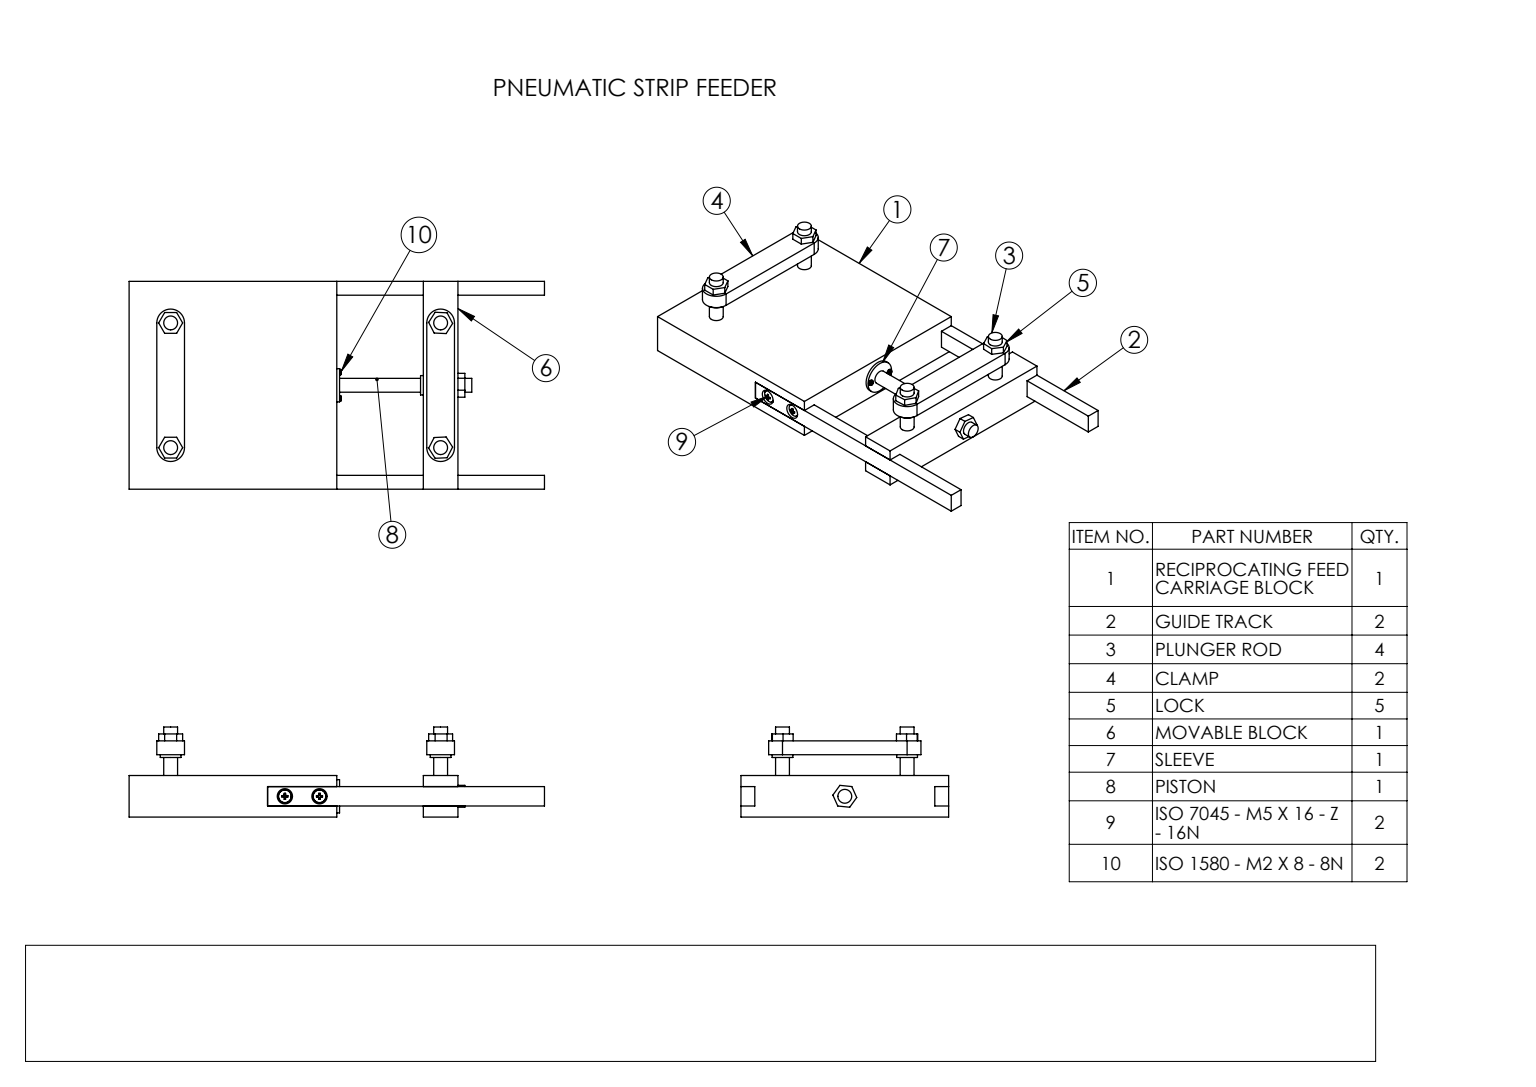
ISO-10303-21;
HEADER;
FILE_DESCRIPTION (('STEP AP214'),
    '1' );
FILE_NAME ('MAS-179',
    '2026-10-27T14:18:53',
    ( '' ),
    ( '' ),
    'SwSTEP 2.0',
    'SolidWorks 2026',
    '' );
FILE_SCHEMA (( 'AUTOMOTIVE_DESIGN' ));
ENDSEC;

DATA;
#1 = DIRECTION ( 'NONE',  ( -1.000000000000000000, -0.000000000000000000, -0.000000000000000000 ) ) ;
#2 = PLANE ( 'NONE',  #2825 ) ;
#3 = LINE ( 'NONE', #3246, #2138 ) ;
#4 = EDGE_LOOP ( 'NONE', ( #1502, #1673, #5385 ) ) ;
#5 = DIRECTION ( 'NONE',  ( -0.02052338132068530496, 0.000000000000000000, 0.9997893732277642886 ) ) ;
#6 = FACE_BOUND ( 'NONE', #2071, .T. ) ;
#7 = AXIS2_PLACEMENT_3D ( 'NONE', #5540, #5177, #924 ) ;
#8 = CARTESIAN_POINT ( 'NONE',  ( 2.740000000000000213, -0.9838866223905674557, -0.5150000000000000133 ) ) ;
#9 = CIRCLE ( 'NONE', #2713, 2.649999999999999467 ) ;
#10 = FACE_OUTER_BOUND ( 'NONE', #5268, .T. ) ;
#11 = COLOUR_RGB ( '',0.8941176470588234615, 0.8941176470588234615, 0.8941176470588234615 ) ;
#12 = AXIS2_PLACEMENT_3D ( 'NONE', #3102, #281, #5829 ) ;
#13 = EDGE_LOOP ( 'NONE', ( #5766, #2705, #5746, #232 ) ) ;
#14 = CARTESIAN_POINT ( 'NONE',  ( 0.000000000000000000, -2.349999999999999201, -0.5150000000000000133 ) ) ;
#15 = CONTEXT_DEPENDENT_SHAPE_REPRESENTATION ( #3045, #4270 ) ;
#16 = AXIS2_PLACEMENT_3D ( 'NONE', #3293, #3357, #1408 ) ;
#17 = DIRECTION ( 'NONE',  ( 1.000000000000000000, -0.000000000000000000, -0.000000000000000000 ) ) ;
#18 = ORIENTED_EDGE ( 'NONE', *, *, #5131, .T. ) ;
#19 = DIRECTION ( 'NONE',  ( 0.8571673013836870192, 1.049727191973306873E-16, -0.5150380737757234151 ) ) ;
#20 = ADVANCED_FACE ( 'NONE', ( #1293 ), #2022, .F. ) ;
#21 = VECTOR ( 'NONE', #291, 1000.000000000000000 ) ;
#22 = EDGE_LOOP ( 'NONE', ( #259, #3713, #2794, #1342 ) ) ;
#23 = ADVANCED_FACE ( 'NONE', ( #3966 ), #1603, .F. ) ;
#24 = ORIENTED_EDGE ( 'NONE', *, *, #4586, .F. ) ;
#25 = CIRCLE ( 'NONE', #2627, 2.500000000000002220 ) ;
#26 = EDGE_CURVE ( 'NONE', #2563, #1725, #4179, .T. ) ;
#27 = TOROIDAL_SURFACE ( 'NONE', #1462, 4.300000000000001599, 0.4499999999999985678 ) ;
#28 = DIRECTION ( 'NONE',  ( 1.000000000000000000, -0.000000000000000000, -0.000000000000000000 ) ) ;
#29 = CARTESIAN_POINT ( 'NONE',  ( 19.70000000000000284, 2.500000000000000000, 0.000000000000000000 ) ) ;
#30 = CARTESIAN_POINT ( 'NONE',  ( 25.00000000000000711, 7.000000000000011546, 65.00000000000000000 ) ) ;
#31 = CARTESIAN_POINT ( 'NONE',  ( 137.4999999999999716, -7.000000000000013323, 75.00000000000001421 ) ) ;
#32 = EDGE_LOOP ( 'NONE', ( #2166, #2925, #468, #4500 ) ) ;
#33 = CIRCLE ( 'NONE', #3411, 2.500000000000002220 ) ;
#34 = VECTOR ( 'NONE', #480, 1000.000000000000000 ) ;
#35 = FILL_AREA_STYLE ('',( #3774 ) ) ;
#36 = CARTESIAN_POINT ( 'NONE',  ( 2.740000000000000213, 0.000000000000000000, 0.8509999999999999787 ) ) ;
#37 = AXIS2_PLACEMENT_3D ( 'NONE', #854, #5957, #5527 ) ;
#38 = SPHERICAL_SURFACE ( 'NONE', #3792, 8.000000000000000000 ) ;
#39 = EDGE_CURVE ( 'NONE', #3671, #1708, #102, .T. ) ;
#40 = MECHANICAL_DESIGN_GEOMETRIC_PRESENTATION_REPRESENTATION (  '', ( #808 ), #5082 ) ;
#41 = ORIENTED_EDGE ( 'NONE', *, *, #5391, .F. ) ;
#42 = DIRECTION ( 'NONE',  ( -1.000000000000000000, -0.000000000000000000, -0.000000000000000000 ) ) ;
#43 = AXIS2_PLACEMENT_3D ( 'NONE', #4617, #1390, #1920 ) ;
#44 = ORIENTED_EDGE ( 'NONE', *, *, #2648, .T. ) ;
#45 = CARTESIAN_POINT ( 'NONE',  ( 55.00000000000000711, 0.000000000000000000, 0.000000000000000000 ) ) ;
#46 = CARTESIAN_POINT ( 'NONE',  ( 0.3226060873438392207, -0.5150000000000068967, 2.189154565102729766 ) ) ;
#47 = ITEM_DEFINED_TRANSFORMATION ( 'NONE', 'NONE', #4502,  #5080 ) ;
#48 = SURFACE_STYLE_USAGE ( .BOTH. , #917 ) ;
#49 = EDGE_LOOP ( 'NONE', ( #4386, #5805, #654, #4968 ) ) ;
#50 = DIRECTION ( 'NONE',  ( -1.000000000000000000, -0.000000000000000000, -0.000000000000000000 ) ) ;
#51 = VERTEX_POINT ( 'NONE', #4696 ) ;
#52 = VERTEX_POINT ( 'NONE', #526 ) ;
#53 =( NAMED_UNIT ( * ) PLANE_ANGLE_UNIT ( ) SI_UNIT ( $, .RADIAN. ) );
#54 = CARTESIAN_POINT ( 'NONE',  ( 0.000000000000000000, 0.000000000000000000, 75.00000000000000000 ) ) ;
#55 = EDGE_CURVE ( 'NONE', #1875, #2958, #1837, .T. ) ;
#56 = CARTESIAN_POINT ( 'NONE',  ( -45.00000000000002842, 0.000000000000000000, -49.99999999999998579 ) ) ;
#57 = DIRECTION ( 'NONE',  ( 0.000000000000000000, 0.000000000000000000, -1.000000000000000000 ) ) ;
#58 = PRODUCT ( 'Reciprocating Feed Carriage Block', 'Reciprocating Feed Carriage Block', '', ( #3675 ) ) ;
#59 = DIRECTION ( 'NONE',  ( 0.000000000000000000, 0.000000000000000000, 1.000000000000000000 ) ) ;
#60 = VERTEX_POINT ( 'NONE', #3659 ) ;
#61 = ADVANCED_FACE ( 'NONE', ( #5096 ), #2836, .F. ) ;
#62 = CARTESIAN_POINT ( 'NONE',  ( 0.000000000000000000, 0.000000000000000000, 0.000000000000000000 ) ) ;
#63 = DIRECTION ( 'NONE',  ( 0.000000000000000000, 1.000000000000000000, 3.280956645156627724E-15 ) ) ;
#64 =( REPRESENTATION_RELATIONSHIP ('NONE','NONE', #5609, #5016 ) REPRESENTATION_RELATIONSHIP_WITH_TRANSFORMATION ( #5642 )SHAPE_REPRESENTATION_RELATIONSHIP( ) );
#65 = AXIS2_PLACEMENT_3D ( 'NONE', #2300, #5491, #4094 ) ;
#66 = DIRECTION ( 'NONE',  ( 1.000000000000000000, 0.000000000000000000, 0.000000000000000000 ) ) ;
#67 = ORIENTED_EDGE ( 'NONE', *, *, #3505, .F. ) ;
#68 =( NAMED_UNIT ( * ) SI_UNIT ( $, .STERADIAN. ) SOLID_ANGLE_UNIT ( ) );
#69 = LINE ( 'NONE', #156, #3339 ) ;
#70 = ADVANCED_FACE ( 'NONE', ( #1406 ), #469, .F. ) ;
#71 = AXIS2_PLACEMENT_3D ( 'NONE', #3867, #5717, #1567 ) ;
#72 = EDGE_LOOP ( 'NONE', ( #5163, #1445, #4342, #1553 ) ) ;
#73 = CARTESIAN_POINT ( 'NONE',  ( 2.740000000000000213, 0.000000000000000000, 0.000000000000000000 ) ) ;
#74 = CARTESIAN_POINT ( 'NONE',  ( -25.39999999999996305, 0.000000000000000000, 0.000000000000000000 ) ) ;
#75 = LINE ( 'NONE', #5584, #2218 ) ;
#76 = CARTESIAN_POINT ( 'NONE',  ( 24.99999999999998224, 6.999999999999985789, 65.00000000000000000 ) ) ;
#77 = ORIENTED_EDGE ( 'NONE', *, *, #5201, .F. ) ;
#78 = ORIENTED_EDGE ( 'NONE', *, *, #4185, .T. ) ;
#79 = PRESENTATION_STYLE_ASSIGNMENT (( #620 ) ) ;
#80 = DIRECTION ( 'NONE',  ( 0.000000000000000000, 1.000000000000000000, -0.000000000000000000 ) ) ;
#81 = ORIENTED_EDGE ( 'NONE', *, *, #5316, .T. ) ;
#82 = DIRECTION ( 'NONE',  ( -1.000000000000000000, -0.000000000000000000, -0.000000000000000000 ) ) ;
#83 = DIRECTION ( 'NONE',  ( 0.000000000000000000, 1.000000000000000000, 0.000000000000000000 ) ) ;
#84 = DIRECTION ( 'NONE',  ( 0.000000000000000000, 0.000000000000000000, 1.000000000000000000 ) ) ;
#85 = ORIENTED_EDGE ( 'NONE', *, *, #3683, .T. ) ;
#86 =( NAMED_UNIT ( * ) PLANE_ANGLE_UNIT ( ) SI_UNIT ( $, .RADIAN. ) );
#87 = DIRECTION ( 'NONE',  ( -0.000000000000000000, -1.000000000000000000, -0.000000000000000000 ) ) ;
#88 = CIRCLE ( 'NONE', #5797, 5.000000000000004441 ) ;
#89 = CARTESIAN_POINT ( 'NONE',  ( -55.00000000000001421, 40.00000000000000000, -45.00000000000000000 ) ) ;
#90 = CARTESIAN_POINT ( 'NONE',  ( 75.00000000000001421, 0.000000000000000000, 0.000000000000000000 ) ) ;
#91 = ADVANCED_FACE ( 'NONE', ( #3214 ), #1319, .F. ) ;
#92 = ORIENTED_EDGE ( 'NONE', *, *, #3018, .T. ) ;
#93 = ADVANCED_FACE ( 'NONE', ( #1832 ), #5149, .T. ) ;
#94 = VERTEX_POINT ( 'NONE', #863 ) ;
#95 = DIRECTION ( 'NONE',  ( -0.000000000000000000, -0.000000000000000000, 1.000000000000000000 ) ) ;
#96 = AXIS2_PLACEMENT_3D ( 'NONE', #2644, #2066, #2156 ) ;
#97 = EDGE_CURVE ( 'NONE', #4020, #2197, #3211, .T. ) ;
#98 = VECTOR ( 'NONE', #2286, 1000.000000000000000 ) ;
#99 = EDGE_LOOP ( 'NONE', ( #5298, #5545, #3236, #2859 ) ) ;
#100 = FACE_OUTER_BOUND ( 'NONE', #830, .T. ) ;
#101 = CARTESIAN_POINT ( 'NONE',  ( 0.06760930072668806801, -4.837354856632045452E-15, 0.000000000000000000 ) ) ;
#102 = CIRCLE ( 'NONE', #5140, 2.500000000000002220 ) ;
#103 = CARTESIAN_POINT ( 'NONE',  ( 1.424271237134740131, 0.000000000000000000, 0.000000000000000000 ) ) ;
#104 = SURFACE_STYLE_FILL_AREA ( #4777 ) ;
#105 = VERTEX_POINT ( 'NONE', #4634 ) ;
#106 = EDGE_CURVE ( 'NONE', #5742, #4738, #1545, .T. ) ;
#107 = VERTEX_POINT ( 'NONE', #2804 ) ;
#108 = AXIS2_PLACEMENT_3D ( 'NONE', #1468, #5154, #2894 ) ;
#109 = LINE ( 'NONE', #3376, #1061 ) ;
#110 = CARTESIAN_POINT ( 'NONE',  ( 7.345657149124971141, -1.312408941149200814, 2.762944903268657774E-16 ) ) ;
#111 = VERTEX_POINT ( 'NONE', #3686 ) ;
#112 = VECTOR ( 'NONE', #1206, 1000.000000000000000 ) ;
#113 = AXIS2_PLACEMENT_3D ( 'NONE', #2260, #4112, #2193 ) ;
#114 = FACE_OUTER_BOUND ( 'NONE', #3648, .T. ) ;
#115 = DIRECTION ( 'NONE',  ( -0.000000000000000000, -0.000000000000000000, 1.000000000000000000 ) ) ;
#116 = DIRECTION ( 'NONE',  ( 1.000000000000000000, -0.000000000000000000, -0.000000000000000000 ) ) ;
#117 = EDGE_LOOP ( 'NONE', ( #4692, #1220, #1894, #1366 ) ) ;
#118 = VECTOR ( 'NONE', #5034, 1000.000000000000000 ) ;
#119 = VECTOR ( 'NONE', #946, 1000.000000000000000 ) ;
#120 = FACE_BOUND ( 'NONE', #3180, .T. ) ;
#121 = DIRECTION ( 'NONE',  ( -1.000000000000000000, 0.000000000000000000, 0.000000000000000000 ) ) ;
#122 = CARTESIAN_POINT ( 'NONE',  ( 135.4999999999999716, 0.000000000000000000, 0.000000000000000000 ) ) ;
#123 = CIRCLE ( 'NONE', #1373, 0.8509999999999999787 ) ;
#125 = CIRCLE ( 'NONE', #3997, 7.000000000000000000 ) ;
#124 = DIRECTION ( 'NONE',  ( 0.000000000000000000, 0.000000000000000000, -1.000000000000000000 ) ) ;
#126 = MANIFOLD_SOLID_BREP ( 'Boss-Extrude2', #2558 ) ;
#127 = EDGE_LOOP ( 'NONE', ( #1000, #825, #2890, #4264 ) ) ;
#128 = VERTEX_POINT ( 'NONE', #4177 ) ;
#129 = DIRECTION ( 'NONE',  ( -0.000000000000000000, -1.000000000000000000, -0.000000000000000000 ) ) ;
#130 = EDGE_CURVE ( 'NONE', #4142, #1478, #3633, .T. ) ;
#131 = EDGE_CURVE ( 'NONE', #60, #666, #9, .T. ) ;
#132 = COLOUR_RGB ( '',1.000000000000000000, 0.9490196078431372140, 0.9098039215686274384 ) ;
#133 = ORIENTED_EDGE ( 'NONE', *, *, #2992, .F. ) ;
#134 = CARTESIAN_POINT ( 'NONE',  ( 77.00000000000001421, 0.000000000000000000, -9.500000000000000000 ) ) ;
#135 = EDGE_CURVE ( 'NONE', #2028, #5067, #3489, .T. ) ;
#136 = CARTESIAN_POINT ( 'NONE',  ( 2.740000000000000213, 0.000000000000000000, 0.000000000000000000 ) ) ;
#137 = CARTESIAN_POINT ( 'NONE',  ( 0.5000000000000000000, 0.2499999999999982792, 2.000000000000001776 ) ) ;
#138 = CYLINDRICAL_SURFACE ( 'NONE', #1374, 5.000000000000004441 ) ;
#139 = EDGE_LOOP ( 'NONE', ( #819, #2768, #3895, #5842 ) ) ;
#140 = VERTEX_POINT ( 'NONE', #4746 ) ;
#141 = EDGE_CURVE ( 'NONE', #5390, #1345, #2004, .T. ) ;
#142 = CARTESIAN_POINT ( 'NONE',  ( 2.740000000000000213, -0.9838866223905676778, 0.5149999999999995692 ) ) ;
#143 = CARTESIAN_POINT ( 'NONE',  ( 0.06760930072668894231, -0.9010842325122859764, 0.5149999999999992362 ) ) ;
#144 = LINE ( 'NONE', #4359, #211 ) ;
#145 = LINE ( 'NONE', #3381, #4186 ) ;
#146 = ORIENTED_EDGE ( 'NONE', *, *, #1899, .T. ) ;
#147 = CLOSED_SHELL ( 'NONE', ( #248, #2661, #5068, #1341, #3720, #5571, #3327, #1429, #4479, #1422, #4024 ) ) ;
#148 = APPLICATION_PROTOCOL_DEFINITION ( 'draft international standard', 'automotive_design', 1998, #5751 ) ;
#149 = CARTESIAN_POINT ( 'NONE',  ( 2.740000000000000213, 0.000000000000000000, 0.000000000000000000 ) ) ;
#150 = DIRECTION ( 'NONE',  ( 0.000000000000000000, 1.000000000000000000, 0.000000000000000000 ) ) ;
#151 = CARTESIAN_POINT ( 'NONE',  ( 75.00000000000001421, 1.224646799147354440E-16, -8.500000000000000000 ) ) ;
#152 = DIRECTION ( 'NONE',  ( -0.000000000000000000, -1.000000000000000000, -0.000000000000000000 ) ) ;
#153 = DIRECTION ( 'NONE',  ( 0.000000000000000000, 0.000000000000000000, 1.000000000000000000 ) ) ;
#154 = EDGE_LOOP ( 'NONE', ( #4564, #1318, #947, #4844 ) ) ;
#155 = ORIENTED_EDGE ( 'NONE', *, *, #5293, .T. ) ;
#156 = CARTESIAN_POINT ( 'NONE',  ( 2.740000000000000213, 0.5150000000000035660, -0.9838866223905657904 ) ) ;
#157 = UNCERTAINTY_MEASURE_WITH_UNIT (LENGTH_MEASURE( 1.000000000000000082E-05 ), #285, 'distance_accuracy_value', 'NONE');
#158 = ORIENTED_EDGE ( 'NONE', *, *, #2741, .F. ) ;
#159 = EDGE_CURVE ( 'NONE', #4312, #626, #169, .T. ) ;
#160 = CARTESIAN_POINT ( 'NONE',  ( 0.6000000000000000888, 0.000000000000000000, 0.000000000000000000 ) ) ;
#161 = CARTESIAN_POINT ( 'NONE',  ( 0.5000000000000000000, 0.2499999999999982792, -2.000000000000000000 ) ) ;
#162 = CONTEXT_DEPENDENT_SHAPE_REPRESENTATION ( #64, #5291 ) ;
#163 = DIRECTION ( 'NONE',  ( 1.000000000000000000, 0.000000000000000000, 0.000000000000000000 ) ) ;
#164 = PRODUCT_RELATED_PRODUCT_CATEGORY ( 'part', '', ( #1927 ) ) ;
#165 = DIRECTION ( 'NONE',  ( 0.000000000000000000, 0.000000000000000000, 1.000000000000000000 ) ) ;
#166 = ORIENTED_EDGE ( 'NONE', *, *, #2504, .F. ) ;
#167 = ORIENTED_EDGE ( 'NONE', *, *, #1148, .F. ) ;
#168 = ADVANCED_FACE ( 'NONE', ( #2861 ), #5707, .F. ) ;
#169 = LINE ( 'NONE', #5681, #675 ) ;
#170 = DIRECTION ( 'NONE',  ( 1.000000000000000000, 0.000000000000000000, 0.000000000000000000 ) ) ;
#171 = VERTEX_POINT ( 'NONE', #3409 ) ;
#172 = DIRECTION ( 'NONE',  ( 0.000000000000000000, 0.000000000000000000, -1.000000000000000000 ) ) ;
#173 = DIRECTION ( 'NONE',  ( -1.000000000000000000, -0.000000000000000000, -0.000000000000000000 ) ) ;
#174 = DIRECTION ( 'NONE',  ( 0.8949343913984706411, 1.487067055422294855E-15, -0.4461977533473793223 ) ) ;
#175 = ORIENTED_EDGE ( 'NONE', *, *, #2979, .F. ) ;
#176 = EDGE_CURVE ( 'NONE', #2634, #3745, #5619, .T. ) ;
#177 = DIRECTION ( 'NONE',  ( 0.9997893732277642886, 0.000000000000000000, -0.02052338132068530496 ) ) ;
#178 = CARTESIAN_POINT ( 'NONE',  ( -53.66025403784439618, 45.00000000000000000, 45.00000000000001421 ) ) ;
#179 = DIRECTION ( 'NONE',  ( 1.000000000000000000, 0.000000000000000000, 0.000000000000000000 ) ) ;
#180 = PLANE ( 'NONE',  #2511 ) ;
#181 = DIRECTION ( 'NONE',  ( 0.000000000000000000, 0.000000000000000000, 1.000000000000000000 ) ) ;
#182 = DIRECTION ( 'NONE',  ( -0.8949343913984706411, 0.4461977533473793223, 0.000000000000000000 ) ) ;
#183 = ORIENTED_EDGE ( 'NONE', *, *, #1823, .F. ) ;
#184 = EDGE_LOOP ( 'NONE', ( #1736, #1918, #2803, #4807 ) ) ;
#185 = AXIS2_PLACEMENT_3D ( 'NONE', #3101, #5825, #5378 ) ;
#186 = DIRECTION ( 'NONE',  ( 0.000000000000000000, 0.000000000000000000, -1.000000000000000000 ) ) ;
#187 = EDGE_LOOP ( 'NONE', ( #1142, #4922, #3638, #5470 ) ) ;
#188=STYLED_ITEM('',(#6006),#2182);
#189 = MANIFOLD_SOLID_BREP ( 'RecessCore', #1492 ) ;
#190 = DIRECTION ( 'NONE',  ( 1.000000000000000000, 0.000000000000000000, 0.000000000000000000 ) ) ;
#191 = CARTESIAN_POINT ( 'NONE',  ( 137.4999999999999716, 15.00000000000000000, 75.00000000000001421 ) ) ;
#192 = ORIENTED_EDGE ( 'NONE', *, *, #4630, .T. ) ;
#193 = ORIENTED_EDGE ( 'NONE', *, *, #1729, .T. ) ;
#194 =( NAMED_UNIT ( * ) SI_UNIT ( $, .STERADIAN. ) SOLID_ANGLE_UNIT ( ) );
#195 = AXIS2_PLACEMENT_3D ( 'NONE', #2672, #1764, #375 ) ;
#196 = MANIFOLD_SOLID_BREP ( 'M2 Clearance Hole1', #4902 ) ;
#197 = CARTESIAN_POINT ( 'NONE',  ( 37.50000000000000711, 6.288372600415927295E-15, 65.00000000000000000 ) ) ;
#198 = EDGE_CURVE ( 'NONE', #4039, #4278, #109, .T. ) ;
#199 = VERTEX_POINT ( 'NONE', #3354 ) ;
#200 = DIRECTION ( 'NONE',  ( -1.000000000000000000, 2.312964634635742895E-17, 0.000000000000000000 ) ) ;
#201 = ADVANCED_FACE ( 'NONE', ( #5199 ), #2031, .F. ) ;
#202 = FACE_OUTER_BOUND ( 'NONE', #385, .T. ) ;
#203 = EDGE_CURVE ( 'NONE', #1147, #2495, #5910, .T. ) ;
#204 = PLANE ( 'NONE',  #1558 ) ;
#205 = AXIS2_PLACEMENT_3D ( 'NONE', #3546, #4367, #1077 ) ;
#206 = ORIENTED_EDGE ( 'NONE', *, *, #4724, .F. ) ;
#207 = DIRECTION ( 'NONE',  ( -0.04608749363411584338, 0.000000000000000000, 0.9989374069132286316 ) ) ;
#208 = ADVANCED_FACE ( 'NONE', ( #1064 ), #1706, .F. ) ;
#209 = LINE ( 'NONE', #2049, #935 ) ;
#210 = TOROIDAL_SURFACE ( 'NONE', #5533, 1.336466033005844434, 0.5999999999999999778 ) ;
#211 = VECTOR ( 'NONE', #2932, 1000.000000000000000 ) ;
#212 = CARTESIAN_POINT ( 'NONE',  ( -53.66025403784439618, 45.00000000000000000, 45.00000000000001421 ) ) ;
#213 = CARTESIAN_POINT ( 'NONE',  ( 0.000000000000000000, -2.349999999999997424, 0.5149999999999992362 ) ) ;
#214 = CARTESIAN_POINT ( 'NONE',  ( 137.4999999999999716, 0.000000000000000000, 5.000000000000000000 ) ) ;
#215 = CYLINDRICAL_SURFACE ( 'NONE', #3221, 5.000000000000004441 ) ;
#216 = MANIFOLD_SOLID_BREP ( 'Slot', #3438 ) ;
#217 = ORIENTED_EDGE ( 'NONE', *, *, #5542, .F. ) ;
#218 = AXIS2_PLACEMENT_3D ( 'NONE', #3417, #2963, #2469 ) ;
#219 = ORIENTED_EDGE ( 'NONE', *, *, #1151, .T. ) ;
#220 = LINE ( 'NONE', #1177, #2270 ) ;
#221 = UNCERTAINTY_MEASURE_WITH_UNIT (LENGTH_MEASURE( 1.000000000000000082E-05 ), #1761, 'distance_accuracy_value', 'NONE');
#222 = VECTOR ( 'NONE', #506, 1000.000000000000000 ) ;
#223 = AXIS2_PLACEMENT_3D ( 'NONE', #4631, #50, #5962 ) ;
#224 = EDGE_CURVE ( 'NONE', #3671, #5354, #1284, .T. ) ;
#225 = VERTEX_POINT ( 'NONE', #2651 ) ;
#226 = VECTOR ( 'NONE', #1143, 1000.000000000000000 ) ;
#227 =( NAMED_UNIT ( * ) PLANE_ANGLE_UNIT ( ) SI_UNIT ( $, .RADIAN. ) );
#228 = VECTOR ( 'NONE', #4642, 1000.000000000000000 ) ;
#229 = CYLINDRICAL_SURFACE ( 'NONE', #96, 5.000000000000000000 ) ;
#230 = FACE_BOUND ( 'NONE', #460, .T. ) ;
#231 = ORIENTED_EDGE ( 'NONE', *, *, #2067, .F. ) ;
#232 = ORIENTED_EDGE ( 'NONE', *, *, #1791, .F. ) ;
#233 = EDGE_CURVE ( 'NONE', #2491, #3368, #3007, .T. ) ;
#234 = DIRECTION ( 'NONE',  ( 0.000000000000000000, 1.000000000000000000, 0.000000000000000000 ) ) ;
#235 = EDGE_LOOP ( 'NONE', ( #5621, #519 ) ) ;
#236 = CARTESIAN_POINT ( 'NONE',  ( 3.699999999999998401, 5.817072295949927426E-16, -4.750000000000000000 ) ) ;
#237 = LINE ( 'NONE', #652, #2519 ) ;
#238 = DIRECTION ( 'NONE',  ( 0.000000000000000000, 1.000000000000000000, -0.000000000000000000 ) ) ;
#239 = CIRCLE ( 'NONE', #3046, 1.037871761867652065 ) ;
#240 = ORIENTED_EDGE ( 'NONE', *, *, #1900, .T. ) ;
#241 = SHAPE_DEFINITION_REPRESENTATION ( #544, #4225 ) ;
#242 = FACE_BOUND ( 'NONE', #235, .T. ) ;
#243 = CLOSED_SHELL ( 'NONE', ( #387, #4012, #859, #4445, #3072, #5289, #5765, #2717, #915, #3857, #5172, #2981, #4882, #2867, #4541, #2097, #5257, #5474, #4624, #721, #3860, #288 ) ) ;
#244 = ADVANCED_FACE ( 'NONE', ( #1649 ), #3949, .T. ) ;
#245 = DIRECTION ( 'NONE',  ( 1.000000000000000000, -0.000000000000000000, -0.000000000000000000 ) ) ;
#246 = DIRECTION ( 'NONE',  ( -0.000000000000000000, -0.000000000000000000, -1.000000000000000000 ) ) ;
#247 = LINE ( 'NONE', #2084, #1072 ) ;
#248 = ADVANCED_FACE ( 'NONE', ( #4015 ), #1620, .F. ) ;
#249 = DIRECTION ( 'NONE',  ( -0.000000000000000000, 0.000000000000000000, -1.000000000000000000 ) ) ;
#250 = EDGE_LOOP ( 'NONE', ( #3367, #4044, #762, #2973 ) ) ;
#251 = ORIENTED_EDGE ( 'NONE', *, *, #3575, .F. ) ;
#252 = CARTESIAN_POINT ( 'NONE',  ( -53.66025403784439618, 40.00000000000000000, 45.00000000000001421 ) ) ;
#253 = ORIENTED_EDGE ( 'NONE', *, *, #2086, .T. ) ;
#254 = ADVANCED_FACE ( 'NONE', ( #5836 ), #1248, .F. ) ;
#255 = LINE ( 'NONE', #2124, #1542 ) ;
#256 = APPLICATION_CONTEXT ( 'automotive_design' ) ;
#257 = CARTESIAN_POINT ( 'NONE',  ( 2.740000000000000213, -0.5150000000000022338, 0.6774776749089210792 ) ) ;
#258 = ORIENTED_EDGE ( 'NONE', *, *, #3702, .T. ) ;
#259 = ORIENTED_EDGE ( 'NONE', *, *, #388, .T. ) ;
#260 = CARTESIAN_POINT ( 'NONE',  ( 67.00000000000001421, 6.123233995736766282E-16, 5.000000000000000000 ) ) ;
#261 = ORIENTED_EDGE ( 'NONE', *, *, #932, .T. ) ;
#262 = DIRECTION ( 'NONE',  ( 1.000000000000000000, -0.000000000000000000, -0.000000000000000000 ) ) ;
#263 = LINE ( 'NONE', #1654, #3890 ) ;
#264 = DIRECTION ( 'NONE',  ( -1.000000000000000000, -0.000000000000000000, -0.000000000000000000 ) ) ;
#265 = ORIENTED_EDGE ( 'NONE', *, *, #3879, .F. ) ;
#266 = CARTESIAN_POINT ( 'NONE',  ( 197.0261205246305281, 0.000000000000000000, -87.87824609756007987 ) ) ;
#267 = CARTESIAN_POINT ( 'NONE',  ( 196.6421356237309510, 0.000000000000000000, 5.000000000000000000 ) ) ;
#268 = CYLINDRICAL_SURFACE ( 'NONE', #4477, 2.500000000000002220 ) ;
#269 = DIRECTION ( 'NONE',  ( 0.000000000000000000, 1.000000000000000000, 1.153406566473941260E-16 ) ) ;
#270 = DIRECTION ( 'NONE',  ( -0.000000000000000000, -1.000000000000000000, -0.000000000000000000 ) ) ;
#271 = CARTESIAN_POINT ( 'NONE',  ( 24.99999999999998224, 6.999999999999985789, 75.00000000000000000 ) ) ;
#272 = MANIFOLD_SOLID_BREP ( 'Cut-Extrude2', #243 ) ;
#273 = ORIENTED_EDGE ( 'NONE', *, *, #4438, .F. ) ;
#274 = ORIENTED_EDGE ( 'NONE', *, *, #5318, .F. ) ;
#275 = DIRECTION ( 'NONE',  ( 0.000000000000000000, 0.000000000000000000, 1.000000000000000000 ) ) ;
#276 = ORIENTED_EDGE ( 'NONE', *, *, #2236, .T. ) ;
#277 = ADVANCED_FACE ( 'NONE', ( #3588 ), #323, .T. ) ;
#278 = EDGE_CURVE ( 'NONE', #1461, #3435, #2305, .T. ) ;
#279 = CARTESIAN_POINT ( 'NONE',  ( 19.70000000000000284, 0.000000000000000000, 2.500000000000000000 ) ) ;
#280 = EDGE_CURVE ( 'NONE', #2788, #5831, #1766, .T. ) ;
#281 = DIRECTION ( 'NONE',  ( 1.000000000000000000, 0.000000000000000000, 0.000000000000000000 ) ) ;
#282 = ORIENTED_EDGE ( 'NONE', *, *, #2831, .T. ) ;
#283 = VERTEX_POINT ( 'NONE', #413 ) ;
#284 = PRESENTATION_STYLE_ASSIGNMENT (( #3561 ) ) ;
#285 =( LENGTH_UNIT ( ) NAMED_UNIT ( * ) SI_UNIT ( .MILLI., .METRE. ) );
#286 = ORIENTED_EDGE ( 'NONE', *, *, #1877, .F. ) ;
#287 = CARTESIAN_POINT ( 'NONE',  ( 0.5000000000000000000, 0.000000000000000000, 0.000000000000000000 ) ) ;
#288 = ADVANCED_FACE ( 'NONE', ( #4164 ), #2769, .F. ) ;
#289 = DIRECTION ( 'NONE',  ( 0.000000000000000000, 0.000000000000000000, 1.000000000000000000 ) ) ;
#290 = ORIENTED_EDGE ( 'NONE', *, *, #4030, .T. ) ;
#291 = DIRECTION ( 'NONE',  ( 1.000000000000000000, -3.469446951953614189E-16, -0.000000000000000000 ) ) ;
#292 = EDGE_LOOP ( 'NONE', ( #561, #1118, #3736, #5489 ) ) ;
#293=STYLED_ITEM('',(#6020),#2209);
#294 = ITEM_DEFINED_TRANSFORMATION ( 'NONE', 'NONE', #43,  #5080 ) ;
#295 = CARTESIAN_POINT ( 'NONE',  ( 0.000000000000000000, -0.2499999999999999445, 1.312875263449798879 ) ) ;
#296 = DIRECTION ( 'NONE',  ( 0.000000000000000000, 0.000000000000000000, -1.000000000000000000 ) ) ;
#297 = COLOUR_RGB ( '',0.8941176470588234615, 0.8941176470588234615, 0.8941176470588234615 ) ;
#298 = VECTOR ( 'NONE', #2052, 1000.000000000000227 ) ;
#299 = FACE_OUTER_BOUND ( 'NONE', #2161, .T. ) ;
#300 = DIRECTION ( 'NONE',  ( -1.000000000000000000, -0.000000000000000000, -0.000000000000000000 ) ) ;
#301 = EDGE_CURVE ( 'NONE', #4985, #4357, #4292, .T. ) ;
#302 = CARTESIAN_POINT ( 'NONE',  ( 1.424271237134740131, 0.000000000000000000, 0.000000000000000000 ) ) ;
#303 = ORIENTED_EDGE ( 'NONE', *, *, #3462, .T. ) ;
#304 = MECHANICAL_DESIGN_GEOMETRIC_PRESENTATION_REPRESENTATION (  '', ( #5611 ), #1259 ) ;
#305 = VECTOR ( 'NONE', #5098, 1000.000000000000000 ) ;
#306 = DIRECTION ( 'NONE',  ( 0.000000000000000000, 0.000000000000000000, 1.000000000000000000 ) ) ;
#307 = ORIENTED_EDGE ( 'NONE', *, *, #4245, .F. ) ;
#308 = AXIS2_PLACEMENT_3D ( 'NONE', #4125, #4984, #3159 ) ;
#309 = DIRECTION ( 'NONE',  ( -0.000000000000000000, -1.000000000000000000, -0.000000000000000000 ) ) ;
#310 = PRESENTATION_STYLE_ASSIGNMENT (( #4469 ) ) ;
#311 = ADVANCED_FACE ( 'NONE', ( #2255 ), #3623, .F. ) ;
#312 = DIRECTION ( 'NONE',  ( 1.000000000000000000, 0.000000000000000000, -0.000000000000000000 ) ) ;
#313 = CIRCLE ( 'NONE', #2040, 7.983406227920510467 ) ;
#314 = AXIS2_PLACEMENT_3D ( 'NONE', #3288, #1427, #2751 ) ;
#315 = EDGE_CURVE ( 'NONE', #2436, #2440, #3153, .T. ) ;
#316 = EDGE_CURVE ( 'NONE', #4485, #2436, #3260, .T. ) ;
#317 = CARTESIAN_POINT ( 'NONE',  ( 137.4999999999999716, 15.00000000000000000, 65.00000000000000000 ) ) ;
#318 = AXIS2_PLACEMENT_3D ( 'NONE', #5107, #1395, #3704 ) ;
#319 = VECTOR ( 'NONE', #2665, 1000.000000000000000 ) ;
#321 = ORIENTED_EDGE ( 'NONE', *, *, #1308, .F. ) ;
#320 = EDGE_CURVE ( 'NONE', #2852, #1334, #3202, .T. ) ;
#322 = ORIENTED_EDGE ( 'NONE', *, *, #1089, .F. ) ;
#323 = PLANE ( 'NONE',  #5550 ) ;
#324 = PRESENTATION_LAYER_ASSIGNMENT (  '', '', ( #5551 ) ) ;
#325 = CARTESIAN_POINT ( 'NONE',  ( -45.00000000000001421, 30.00000000000000355, -50.00000000000000000 ) ) ;
#326 = ORIENTED_EDGE ( 'NONE', *, *, #3762, .T. ) ;
#327 = DIRECTION ( 'NONE',  ( 0.000000000000000000, 0.000000000000000000, 1.000000000000000000 ) ) ;
#328 = DIRECTION ( 'NONE',  ( 1.000000000000000000, -0.000000000000000000, -0.000000000000000000 ) ) ;
#329 = EDGE_LOOP ( 'NONE', ( #3488, #1309 ) ) ;
#330 = CARTESIAN_POINT ( 'NONE',  ( 8.300922883092140858E-17, -0.2499999999999997780, -1.455170506525537588 ) ) ;
#331 = ORIENTED_EDGE ( 'NONE', *, *, #2483, .F. ) ;
#332 =( GEOMETRIC_REPRESENTATION_CONTEXT ( 3 ) GLOBAL_UNCERTAINTY_ASSIGNED_CONTEXT ( ( #1483 ) ) GLOBAL_UNIT_ASSIGNED_CONTEXT ( ( #2789, #1481, #68 ) ) REPRESENTATION_CONTEXT ( 'NONE', 'WORKASPACE' ) );
#333 = EDGE_CURVE ( 'NONE', #4738, #5742, #4095, .T. ) ;
#334 = ADVANCED_FACE ( 'NONE', ( #4537 ), #4626, .F. ) ;
#335 = DIRECTION ( 'NONE',  ( -0.8660254037844390407, 0.000000000000000000, -0.4999999999999993894 ) ) ;
#336 = AXIS2_PLACEMENT_3D ( 'NONE', #1876, #5603, #1027 ) ;
#337 = CARTESIAN_POINT ( 'NONE',  ( 2.740000000000000213, -0.5149999999999961275, -0.9838866223905694541 ) ) ;
#338 = AXIS2_PLACEMENT_3D ( 'NONE', #4886, #3449, #2991 ) ;
#339 = DIRECTION ( 'NONE',  ( 1.000000000000000000, 0.000000000000000000, 0.000000000000000000 ) ) ;
#340 = LINE ( 'NONE', #5874, #5255 ) ;
#341 = DIRECTION ( 'NONE',  ( -1.000000000000000000, -0.000000000000000000, -0.000000000000000000 ) ) ;
#342 = VERTEX_POINT ( 'NONE', #46 ) ;
#343 = CARTESIAN_POINT ( 'NONE',  ( 68.00000000000000000, -1.951563910473909559E-15, 75.00000000000000000 ) ) ;
#344 = ORIENTED_EDGE ( 'NONE', *, *, #547, .F. ) ;
#345 = DIRECTION ( 'NONE',  ( -0.000000000000000000, 1.000000000000000000, 1.224646799147353207E-16 ) ) ;
#346 = SHAPE_REPRESENTATION_RELATIONSHIP ( 'NONE' , 'NONE' ,  #2785, #5722 ) ;
#347 = CARTESIAN_POINT ( 'NONE',  ( 2.740000000000000213, 0.9838866223909998876, -0.5150000000000000133 ) ) ;
#348 = FACE_BOUND ( 'NONE', #3880, .T. ) ;
#349 = ADVANCED_FACE ( 'NONE', ( #2746 ), #3674, .F. ) ;
#350 = ORIENTED_EDGE ( 'NONE', *, *, #5483, .F. ) ;
#351 = ORIENTED_EDGE ( 'NONE', *, *, #1899, .F. ) ;
#352 = DIRECTION ( 'NONE',  ( -1.000000000000000000, 0.000000000000000000, 0.000000000000000000 ) ) ;
#353 = DIRECTION ( 'NONE',  ( -0.000000000000000000, -0.000000000000000000, 1.000000000000000000 ) ) ;
#354 = EDGE_LOOP ( 'NONE', ( #2724, #1394 ) ) ;
#355 = CARTESIAN_POINT ( 'NONE',  ( -45.00000000000001421, 40.00000000000000000, 50.00000000000000000 ) ) ;
#356 = CARTESIAN_POINT ( 'NONE',  ( -74.99999999999998579, 15.00000000000000000, 75.00000000000000000 ) ) ;
#357 = ORIENTED_EDGE ( 'NONE', *, *, #4065, .T. ) ;
#358 = DIRECTION ( 'NONE',  ( 0.000000000000000000, 0.000000000000000000, -1.000000000000000000 ) ) ;
#359 = ADVANCED_FACE ( 'NONE', ( #1881 ), #3735, .T. ) ;
#360 = VERTEX_POINT ( 'NONE', #5089 ) ;
#361 = AXIS2_PLACEMENT_3D ( 'NONE', #2845, #4273, #538 ) ;
#362 = DIRECTION ( 'NONE',  ( 0.000000000000000000, 0.000000000000000000, 1.000000000000000000 ) ) ;
#363 = DIRECTION ( 'NONE',  ( 0.000000000000000000, 0.000000000000000000, 1.000000000000000000 ) ) ;
#364 = AXIS2_PLACEMENT_3D ( 'NONE', #2626, #335, #1690 ) ;
#365 = DIRECTION ( 'NONE',  ( -0.000000000000000000, -0.000000000000000000, 1.000000000000000000 ) ) ;
#366 = DIRECTION ( 'NONE',  ( -1.000000000000000000, -0.000000000000000000, -0.000000000000000000 ) ) ;
#367 = EDGE_CURVE ( 'NONE', #1773, #5556, #4512, .T. ) ;
#368 = EDGE_LOOP ( 'NONE', ( #4286, #2908, #2582, #3247 ) ) ;
#369 = CARTESIAN_POINT ( 'NONE',  ( -45.00000000000002842, 15.00000000000000000, -39.99999999999997868 ) ) ;
#370 = ORIENTED_EDGE ( 'NONE', *, *, #3462, .F. ) ;
#371 = DIRECTION ( 'NONE',  ( -1.000000000000000000, -0.000000000000000000, -0.000000000000000000 ) ) ;
#372 = ADVANCED_FACE ( 'NONE', ( #1311 ), #889, .T. ) ;
#373 = FILL_AREA_STYLE ('',( #5951 ) ) ;
#374 = CYLINDRICAL_SURFACE ( 'NONE', #2638, 4.749999999999999112 ) ;
#375 = DIRECTION ( 'NONE',  ( 0.000000000000000000, 0.000000000000000000, -1.000000000000000000 ) ) ;
#376 = EDGE_LOOP ( 'NONE', ( #1948, #3141, #4446, #529, #3460, #5164, #2752, #3738, #499, #1793, #4023, #3829 ) ) ;
#377 = VERTEX_POINT ( 'NONE', #441 ) ;
#378 = CARTESIAN_POINT ( 'NONE',  ( -53.66025403784439618, 45.00000000000000000, 45.00000000000001421 ) ) ;
#379 = ORIENTED_EDGE ( 'NONE', *, *, #3057, .F. ) ;
#380 = DIRECTION ( 'NONE',  ( -3.469446951953614189E-16, -1.000000000000000000, 8.673617379884041635E-17 ) ) ;
#381 = CARTESIAN_POINT ( 'NONE',  ( 150.0000000000000284, 15.00000000000000000, 45.00000000000000000 ) ) ;
#382 = ORIENTED_EDGE ( 'NONE', *, *, #3138, .T. ) ;
#383 = LINE ( 'NONE', #2712, #21 ) ;
#384 = ORIENTED_EDGE ( 'NONE', *, *, #5078, .T. ) ;
#385 = EDGE_LOOP ( 'NONE', ( #2934, #576, #5503, #570 ) ) ;
#386 = VECTOR ( 'NONE', #1556, 1000.000000000000000 ) ;
#387 = ADVANCED_FACE ( 'NONE', ( #827 ), #2284, .F. ) ;
#388 = EDGE_CURVE ( 'NONE', #475, #702, #3140, .T. ) ;
#389 = CARTESIAN_POINT ( 'NONE',  ( 25.00000000000000711, 7.000000000000011546, -75.00000000000000000 ) ) ;
#390 = EDGE_CURVE ( 'NONE', #5094, #2958, #1969, .T. ) ;
#391 = DIRECTION ( 'NONE',  ( -0.000000000000000000, -0.000000000000000000, 1.000000000000000000 ) ) ;
#392 = CARTESIAN_POINT ( 'NONE',  ( 137.4999999999999716, 15.00000000000000000, -75.00000000000000000 ) ) ;
#393 = DIRECTION ( 'NONE',  ( 0.000000000000000000, 0.000000000000000000, -1.000000000000000000 ) ) ;
#394=STYLED_ITEM('',(#6013),#2189);
#395 = EDGE_LOOP ( 'NONE', ( #4054, #2100 ) ) ;
#396 = EDGE_CURVE ( 'NONE', #4357, #4985, #5381, .T. ) ;
#397 = SHAPE_REPRESENTATION_RELATIONSHIP ( 'NONE' , 'NONE' ,  #951, #4058 ) ;
#398 = DIRECTION ( 'NONE',  ( 1.000000000000000000, -0.000000000000000000, -0.000000000000000000 ) ) ;
#399 = AXIS2_PLACEMENT_3D ( 'NONE', #949, #5510, #3267 ) ;
#400 = VECTOR ( 'NONE', #539, 1000.000000000000000 ) ;
#401 = ORIENTED_EDGE ( 'NONE', *, *, #5953, .F. ) ;
#402 = FACE_BOUND ( 'NONE', #4375, .T. ) ;
#403 = AXIS2_PLACEMENT_3D ( 'NONE', #4521, #1, #363 ) ;
#404 = LINE ( 'NONE', #5952, #3410 ) ;
#405 = EDGE_CURVE ( 'NONE', #1403, #3083, #5296, .T. ) ;
#406 = VECTOR ( 'NONE', #2782, 1000.000000000000000 ) ;
#407 = CIRCLE ( 'NONE', #1166, 5.000000000000004441 ) ;
#408 = FACE_BOUND ( 'NONE', #3152, .T. ) ;
#409 = ORIENTED_EDGE ( 'NONE', *, *, #2019, .F. ) ;
#410 = ORIENTED_EDGE ( 'NONE', *, *, #1827, .F. ) ;
#411 = VECTOR ( 'NONE', #264, 1000.000000000000000 ) ;
#412 = CIRCLE ( 'NONE', #978, 5.000000000000004441 ) ;
#413 = CARTESIAN_POINT ( 'NONE',  ( 62.50000000000001421, -1.951563910473909559E-15, -53.49784845693390167 ) ) ;
#414 = DIRECTION ( 'NONE',  ( -1.000000000000000000, -0.000000000000000000, -0.000000000000000000 ) ) ;
#415 = ORIENTED_EDGE ( 'NONE', *, *, #26, .F. ) ;
#416 = AXIS2_PLACEMENT_3D ( 'NONE', #5969, #3664, #3218 ) ;
#417 = VECTOR ( 'NONE', #1999, 1000.000000000000000 ) ;
#418 = FACE_OUTER_BOUND ( 'NONE', #802, .T. ) ;
#419 = DIRECTION ( 'NONE',  ( 0.000000000000000000, 1.000000000000000000, 0.000000000000000000 ) ) ;
#420 = ORIENTED_EDGE ( 'NONE', *, *, #1641, .T. ) ;
#421 = CARTESIAN_POINT ( 'NONE',  ( 0.05011565059742434380, 0.2499999999999982792, -1.595010514166263382 ) ) ;
#422 = EDGE_LOOP ( 'NONE', ( #5932, #2408, #3611, #5800 ) ) ;
#423 = DIRECTION ( 'NONE',  ( -1.000000000000000000, -0.000000000000000000, -0.000000000000000000 ) ) ;
#424 = CARTESIAN_POINT ( 'NONE',  ( -45.00000000000001421, 50.00000000000000000, 50.00000000000000000 ) ) ;
#425 = CARTESIAN_POINT ( 'NONE',  ( 150.0000000000000284, 15.00000000000000000, -49.99999999999998579 ) ) ;
#426 = CARTESIAN_POINT ( 'NONE',  ( 24.99999999999998224, 6.999999999999985789, 75.00000000000000000 ) ) ;
#427 = CYLINDRICAL_SURFACE ( 'NONE', #3498, 5.000000000000004441 ) ;
#428 = ORIENTED_EDGE ( 'NONE', *, *, #4995, .T. ) ;
#429 = ADVANCED_FACE ( 'NONE', ( #3884 ), #4687, .T. ) ;
#430 =( LENGTH_UNIT ( ) NAMED_UNIT ( * ) SI_UNIT ( .MILLI., .METRE. ) );
#431 = CARTESIAN_POINT ( 'NONE',  ( 1.849560077140108394, 0.7556913915602446741, 0.5149999999999996803 ) ) ;
#432 = PRODUCT_DEFINITION_FORMATION_WITH_SPECIFIED_SOURCE ( 'ANY', '', #4798, .NOT_KNOWN. ) ;
#433 = EDGE_LOOP ( 'NONE', ( #3649, #3374, #834, #5095, #5451 ) ) ;
#434 = CARTESIAN_POINT ( 'NONE',  ( -45.00000000000001421, 40.00000000000000000, 39.99999999999999289 ) ) ;
#435 = AXIS2_PLACEMENT_3D ( 'NONE', #5878, #3224, #2274 ) ;
#436 = CARTESIAN_POINT ( 'NONE',  ( 62.50000000000001421, -1.951563910473909559E-15, -65.00000000000000000 ) ) ;
#437 = CARTESIAN_POINT ( 'NONE',  ( 137.4999999999999716, 6.999999999999985789, 75.00000000000000000 ) ) ;
#438 = ORIENTED_EDGE ( 'NONE', *, *, #2529, .F. ) ;
#439 = EDGE_CURVE ( 'NONE', #128, #2057, #2951, .T. ) ;
#440 = EDGE_LOOP ( 'NONE', ( #5310, #2912, #92, #4963 ) ) ;
#441 = CARTESIAN_POINT ( 'NONE',  ( -45.00000000000001421, 40.00000000000000000, 50.00000000000000000 ) ) ;
#442 = ITEM_DEFINED_TRANSFORMATION ( 'NONE', 'NONE', #1093,  #5080 ) ;
#443 = CARTESIAN_POINT ( 'NONE',  ( 2.740000000000000213, -0.5150000000000034550, 0.9838866223909985553 ) ) ;
#444 = ORIENTED_EDGE ( 'NONE', *, *, #5201, .T. ) ;
#445 = DIRECTION ( 'NONE',  ( -0.000000000000000000, -0.000000000000000000, 1.000000000000000000 ) ) ;
#446 = CARTESIAN_POINT ( 'NONE',  ( 0.06760930072668806801, -4.837354856632045452E-15, 0.000000000000000000 ) ) ;
#447 = ORIENTED_EDGE ( 'NONE', *, *, #1010, .T. ) ;
#448 = EDGE_LOOP ( 'NONE', ( #5357, #973 ) ) ;
#449 = PLANE ( 'NONE',  #1541 ) ;
#450 = CARTESIAN_POINT ( 'NONE',  ( 0.3600944671415647891, -0.2500000000000000000, 1.887947737020718941 ) ) ;
#451 = PLANE ( 'NONE',  #1857 ) ;
#452 = DIRECTION ( 'NONE',  ( -0.000000000000000000, -0.000000000000000000, -1.000000000000000000 ) ) ;
#453 = ORIENTED_EDGE ( 'NONE', *, *, #824, .F. ) ;
#454 = FACE_OUTER_BOUND ( 'NONE', #672, .T. ) ;
#455 = FACE_OUTER_BOUND ( 'NONE', #872, .T. ) ;
#456 = VECTOR ( 'NONE', #5335, 1000.000000000000000 ) ;
#457 = DIRECTION ( 'NONE',  ( -0.000000000000000000, -0.000000000000000000, 1.000000000000000000 ) ) ;
#458 = EDGE_CURVE ( 'NONE', #1563, #1071, #2378, .T. ) ;
#459 = ADVANCED_FACE ( 'NONE', ( #1056 ), #3071, .F. ) ;
#460 = EDGE_LOOP ( 'NONE', ( #331, #4146 ) ) ;
#461 = EDGE_CURVE ( 'NONE', #5479, #5285, #3793, .T. ) ;
#462 = CARTESIAN_POINT ( 'NONE',  ( 172.5000000000000284, 15.00000000000000000, 75.00000000000001421 ) ) ;
#463 = ITEM_DEFINED_TRANSFORMATION ( 'NONE', 'NONE', #3806,  #5080 ) ;
#464 = DIRECTION ( 'NONE',  ( 0.000000000000000000, 0.000000000000000000, -1.000000000000000000 ) ) ;
#465 = ORIENTED_EDGE ( 'NONE', *, *, #3725, .F. ) ;
#466 = DIRECTION ( 'NONE',  ( -1.000000000000000000, 0.000000000000000000, 0.000000000000000000 ) ) ;
#467 = VERTEX_POINT ( 'NONE', #1515 ) ;
#468 = ORIENTED_EDGE ( 'NONE', *, *, #5761, .F. ) ;
#469 = CYLINDRICAL_SURFACE ( 'NONE', #580, 5.000000000000004441 ) ;
#470 = ADVANCED_FACE ( 'NONE', ( #2397 ), #5641, .F. ) ;
#471 = DIRECTION ( 'NONE',  ( 0.000000000000000000, 0.000000000000000000, -1.000000000000000000 ) ) ;
#472 = DIRECTION ( 'NONE',  ( 1.000000000000000000, 0.000000000000000000, 0.000000000000000000 ) ) ;
#473 = DIRECTION ( 'NONE',  ( 0.000000000000000000, 1.000000000000000000, 0.000000000000000000 ) ) ;
#474 = LINE ( 'NONE', #5100, #406 ) ;
#475 = VERTEX_POINT ( 'NONE', #614 ) ;
#476 = CIRCLE ( 'NONE', #7, 5.000000000000004441 ) ;
#477 = DIRECTION ( 'NONE',  ( 0.04608749363411584338, 0.000000000000000000, 0.9989374069132286316 ) ) ;
#478 = CARTESIAN_POINT ( 'NONE',  ( 55.00000000000000711, 0.000000000000000000, 5.000000000000000000 ) ) ;
#479 = VECTOR ( 'NONE', #645, 1000.000000000000000 ) ;
#480 = DIRECTION ( 'NONE',  ( 1.000000000000000000, -3.469446951953614189E-16, 0.000000000000000000 ) ) ;
#482 = ORIENTED_EDGE ( 'NONE', *, *, #2535, .F. ) ;
#481 = PRODUCT_DEFINITION_SHAPE ( 'NONE', 'NONE',  #3494 ) ;
#483 = SURFACE_STYLE_USAGE ( .BOTH. , #3752 ) ;
#484 = CONICAL_SURFACE ( 'NONE', #5051, 2.500000000000002220, 1.029744260000002631 ) ;
#485 = CARTESIAN_POINT ( 'NONE',  ( 77.00000000000001421, 0.000000000000000000, -9.500000000000000000 ) ) ;
#486 = AXIS2_PLACEMENT_3D ( 'NONE', #2448, #4210, #5240 ) ;
#487 = EDGE_LOOP ( 'NONE', ( #1577, #4433, #2223, #5314 ) ) ;
#488 = DIRECTION ( 'NONE',  ( 1.000000000000000000, 0.000000000000000000, 0.000000000000000000 ) ) ;
#489 = DIRECTION ( 'NONE',  ( -0.3090169943749412895, 0.000000000000000000, 0.9510565162951555296 ) ) ;
#490 = ITEM_DEFINED_TRANSFORMATION ( 'NONE', 'NONE', #1961,  #5080 ) ;
#491 = EDGE_CURVE ( 'NONE', #4174, #2799, #3555, .T. ) ;
#492 = AXIS2_PLACEMENT_3D ( 'NONE', #4843, #5206, #1562 ) ;
#493 = CIRCLE ( 'NONE', #4373, 1.099999999999998535 ) ;
#494 = PRODUCT ( 'sleeve', 'sleeve', '', ( #2080 ) ) ;
#495 = ORIENTED_EDGE ( 'NONE', *, *, #5762, .T. ) ;
#496 = EDGE_CURVE ( 'NONE', #1071, #4278, #5299, .T. ) ;
#497 = CARTESIAN_POINT ( 'NONE',  ( 0.000000000000000000, -0.2499999999999998335, -1.312875263449798879 ) ) ;
#498 = CIRCLE ( 'NONE', #1367, 1.099999999999998535 ) ;
#499 = ORIENTED_EDGE ( 'NONE', *, *, #2236, .F. ) ;
#500 = VERTEX_POINT ( 'NONE', #5168 ) ;
#501 = DIRECTION ( 'NONE',  ( 1.000000000000000000, -0.000000000000000000, -0.000000000000000000 ) ) ;
#502 = VECTOR ( 'NONE', #1263, 1000.000000000000000 ) ;
#503 = VECTOR ( 'NONE', #5031, 1000.000000000000000 ) ;
#504 = DIRECTION ( 'NONE',  ( -1.000000000000000000, -0.000000000000000000, -0.000000000000000000 ) ) ;
#505 = PLANE ( 'NONE',  #2514 ) ;
#506 = DIRECTION ( 'NONE',  ( 0.000000000000000000, -1.000000000000000000, -1.652937667529658626E-16 ) ) ;
#507 = FACE_OUTER_BOUND ( 'NONE', #3343, .T. ) ;
#508 = ORIENTED_EDGE ( 'NONE', *, *, #4349, .F. ) ;
#509 = ADVANCED_FACE ( 'NONE', ( #3345 ), #2461, .T. ) ;
#510 = CARTESIAN_POINT ( 'NONE',  ( 0.6000000000000000888, 1.636698849489768475E-16, -1.336466033005844434 ) ) ;
#511 = PRESENTATION_LAYER_ASSIGNMENT (  '', '', ( #808 ) ) ;
#512 = CARTESIAN_POINT ( 'NONE',  ( 75.00000000000001421, 6.999999999999993783, 65.00000000000000000 ) ) ;
#513 = DIRECTION ( 'NONE',  ( -0.000000000000000000, -0.000000000000000000, 1.000000000000000000 ) ) ;
#514 = EDGE_LOOP ( 'NONE', ( #4207, #2897 ) ) ;
#515 = PRODUCT_CONTEXT ( 'NONE', #5629, 'mechanical' ) ;
#516 = DIRECTION ( 'NONE',  ( 0.000000000000000000, -3.491481338843133355E-15, 1.000000000000000000 ) ) ;
#517 = AXIS2_PLACEMENT_3D ( 'NONE', #14, #3233, #5026 ) ;
#518 = AXIS2_PLACEMENT_3D ( 'NONE', #4463, #3550, #3968 ) ;
#519 = ORIENTED_EDGE ( 'NONE', *, *, #2394, .F. ) ;
#520 = CYLINDRICAL_SURFACE ( 'NONE', #602, 7.000000000000000000 ) ;
#521 = DIRECTION ( 'NONE',  ( -1.000000000000000000, -0.000000000000000000, -0.000000000000000000 ) ) ;
#522 = CONTEXT_DEPENDENT_SHAPE_REPRESENTATION ( #2103, #5612 ) ;
#523 = DIRECTION ( 'NONE',  ( 0.000000000000000000, -0.000000000000000000, 1.000000000000000000 ) ) ;
#524 = ORIENTED_EDGE ( 'NONE', *, *, #4694, .F. ) ;
#525 = VERTEX_POINT ( 'NONE', #3821 ) ;
#526 = CARTESIAN_POINT ( 'NONE',  ( -40.66987298107781612, 40.00000000000000000, 37.50000000000000000 ) ) ;
#527 = DIRECTION ( 'NONE',  ( 0.000000000000000000, 0.000000000000000000, 1.000000000000000000 ) ) ;
#528 = EDGE_CURVE ( 'NONE', #4999, #2390, #5702, .T. ) ;
#529 = ORIENTED_EDGE ( 'NONE', *, *, #5643, .T. ) ;
#530 = CARTESIAN_POINT ( 'NONE',  ( 77.00000000000001421, 0.000000000000000000, 0.000000000000000000 ) ) ;
#531 = EDGE_CURVE ( 'NONE', #1773, #105, #641, .T. ) ;
#532 = DIRECTION ( 'NONE',  ( -0.000000000000000000, -1.000000000000000000, -0.000000000000000000 ) ) ;
#533 = PRODUCT_DEFINITION_SHAPE ( 'NONE', 'NONE',  #5983 ) ;
#534 = DIRECTION ( 'NONE',  ( 0.000000000000000000, 0.000000000000000000, -1.000000000000000000 ) ) ;
#535 = EDGE_LOOP ( 'NONE', ( #1085, #4060 ) ) ;
#536 = DIRECTION ( 'NONE',  ( 0.000000000000000000, 0.000000000000000000, 1.000000000000000000 ) ) ;
#537 = EDGE_CURVE ( 'NONE', #199, #3078, #839, .T. ) ;
#538 = DIRECTION ( 'NONE',  ( 0.000000000000000000, 0.000000000000000000, -1.000000000000000000 ) ) ;
#539 = DIRECTION ( 'NONE',  ( 0.8571673013836870192, 1.049727191973306873E-16, -0.5150380737757234151 ) ) ;
#540 = ADVANCED_FACE ( 'NONE', ( #2030 ), #4290, .F. ) ;
#541 = DIRECTION ( 'NONE',  ( 0.000000000000000000, 0.000000000000000000, 1.000000000000000000 ) ) ;
#542 = VERTEX_POINT ( 'NONE', #968 ) ;
#543 = EDGE_LOOP ( 'NONE', ( #1731, #977, #5859, #3323 ) ) ;
#544 = PRODUCT_DEFINITION_SHAPE ( 'NONE', 'NONE',  #3311 ) ;
#545 = DIRECTION ( 'NONE',  ( 0.000000000000000000, 0.000000000000000000, -1.000000000000000000 ) ) ;
#546 = B_SPLINE_CURVE_WITH_KNOTS ( 'NONE', 3,
 ( #5885, #4533, #5083, #2790 ),
 .UNSPECIFIED., .F., .F.,
 ( 4, 4 ),
 ( 0.001586480563516618056, 0.004268227385920363680 ),
 .UNSPECIFIED. ) ;
#547 = EDGE_CURVE ( 'NONE', #3406, #1861, #2828, .T. ) ;
#548 = ORIENTED_EDGE ( 'NONE', *, *, #5422, .F. ) ;
#549 = DIRECTION ( 'NONE',  ( -1.000000000000000000, -0.000000000000000000, -0.000000000000000000 ) ) ;
#550 = DIRECTION ( 'NONE',  ( -0.000000000000000000, -0.000000000000000000, 1.000000000000000000 ) ) ;
#551 = CONTEXT_DEPENDENT_SHAPE_REPRESENTATION ( #1718, #4857 ) ;
#552 = DIRECTION ( 'NONE',  ( -1.000000000000000000, -0.000000000000000000, -0.000000000000000000 ) ) ;
#553 = VERTEX_POINT ( 'NONE', #279 ) ;
#554 = VERTEX_POINT ( 'NONE', #5768 ) ;
#555 = APPLICATION_CONTEXT ( 'automotive_design' ) ;
#556 =( LENGTH_UNIT ( ) NAMED_UNIT ( * ) SI_UNIT ( .MILLI., .METRE. ) );
#557 = DIRECTION ( 'NONE',  ( 0.000000000000000000, 0.000000000000000000, 1.000000000000000000 ) ) ;
#558 = DIRECTION ( 'NONE',  ( 0.5150380737757185301, 0.000000000000000000, -0.8571673013836900168 ) ) ;
#559 = DIRECTION ( 'NONE',  ( 0.000000000000000000, 1.000000000000000000, 0.000000000000000000 ) ) ;
#560 = CARTESIAN_POINT ( 'NONE',  ( -40.66987298107781612, 45.00000000000000000, 37.50000000000000000 ) ) ;
#561 = ORIENTED_EDGE ( 'NONE', *, *, #2602, .F. ) ;
#562 = EDGE_CURVE ( 'NONE', #4905, #467, #1144, .T. ) ;
#563 = DIRECTION ( 'NONE',  ( 1.000000000000000000, 0.000000000000000000, 0.000000000000000000 ) ) ;
#564 = FACE_OUTER_BOUND ( 'NONE', #4940, .T. ) ;
#565 = EDGE_CURVE ( 'NONE', #3630, #140, #2691, .T. ) ;
#566 = DIRECTION ( 'NONE',  ( -0.000000000000000000, -0.000000000000000000, 1.000000000000000000 ) ) ;
#567 = EDGE_CURVE ( 'NONE', #1705, #3162, #5290, .T. ) ;
#568 = DIRECTION ( 'NONE',  ( 0.000000000000000000, -1.734723475976808080E-16, 1.000000000000000000 ) ) ;
#569 = ORIENTED_EDGE ( 'NONE', *, *, #1573, .F. ) ;
#570 = ORIENTED_EDGE ( 'NONE', *, *, #1866, .T. ) ;
#571 =( NAMED_UNIT ( * ) SI_UNIT ( $, .STERADIAN. ) SOLID_ANGLE_UNIT ( ) );
#572 = CARTESIAN_POINT ( 'NONE',  ( 62.50000000000001421, -1.951563910473909559E-15, 65.00000000000000000 ) ) ;
#573 = UNCERTAINTY_MEASURE_WITH_UNIT (LENGTH_MEASURE( 1.000000000000000082E-05 ), #1086, 'distance_accuracy_value', 'NONE');
#574 = CIRCLE ( 'NONE', #1347, 2.500000000000002220 ) ;
#575 = AXIS2_PLACEMENT_3D ( 'NONE', #1998, #3850, #3404 ) ;
#576 = ORIENTED_EDGE ( 'NONE', *, *, #439, .T. ) ;
#577 = FACE_OUTER_BOUND ( 'NONE', #2183, .T. ) ;
#578 = EDGE_CURVE ( 'NONE', #1123, #2345, #5796, .T. ) ;
#579 = DIRECTION ( 'NONE',  ( 0.000000000000000000, 3.490239007934759657E-15, -1.000000000000000000 ) ) ;
#580 = AXIS2_PLACEMENT_3D ( 'NONE', #923, #899, #1346 ) ;
#581 = PRODUCT_DEFINITION_SHAPE ( 'NONE', 'NONE',  #5975 ) ;
#582 = CIRCLE ( 'NONE', #3972, 5.000000000000004441 ) ;
#583 = FACE_OUTER_BOUND ( 'NONE', #5588, .T. ) ;
#584 = CARTESIAN_POINT ( 'NONE',  ( 67.00000000000001421, 0.000000000000000000, 0.000000000000000000 ) ) ;
#585 = ORIENTED_EDGE ( 'NONE', *, *, #2005, .F. ) ;
#586 = ORIENTED_EDGE ( 'NONE', *, *, #4414, .F. ) ;
#587 = CIRCLE ( 'NONE', #1933, 1.099999999999998535 ) ;
#588 = DIRECTION ( 'NONE',  ( -0.000000000000000000, -1.000000000000000000, -0.000000000000000000 ) ) ;
#589 = ORIENTED_EDGE ( 'NONE', *, *, #2162, .T. ) ;
#590 = AXIS2_PLACEMENT_3D ( 'NONE', #4311, #4369, #5694 ) ;
#591 = CIRCLE ( 'NONE', #1662, 7.983406227920510467 ) ;
#592 = LINE ( 'NONE', #3245, #305 ) ;
#593 = DIRECTION ( 'NONE',  ( 0.5000000000000004441, 0.000000000000000000, 0.8660254037844383745 ) ) ;
#594 = DIRECTION ( 'NONE',  ( 1.000000000000000000, -0.000000000000000000, -0.000000000000000000 ) ) ;
#595 = ORIENTED_EDGE ( 'NONE', *, *, #233, .F. ) ;
#596 = PRODUCT_CONTEXT ( 'NONE', #256, 'mechanical' ) ;
#597 = AXIS2_PLACEMENT_3D ( 'NONE', #715, #5362, #4077 ) ;
#598 = CARTESIAN_POINT ( 'NONE',  ( 2.740000000000000213, -0.5150000000000034550, 0.9838866223909985553 ) ) ;
#599 = EDGE_CURVE ( 'NONE', #3899, #5382, #1521, .T. ) ;
#600 = CARTESIAN_POINT ( 'NONE',  ( 40.00000000000000711, 6.594534300202765954E-15, -55.00000000000000000 ) ) ;
#601 = PLANE ( 'NONE',  #5069 ) ;
#602 = AXIS2_PLACEMENT_3D ( 'NONE', #45, #5111, #4256 ) ;
#604 = VECTOR ( 'NONE', #4156, 1000.000000000000000 ) ;
#603 = DIRECTION ( 'NONE',  ( 0.8571673013836870192, 0.000000000000000000, 0.5150380737757234151 ) ) ;
#605 = VERTEX_POINT ( 'NONE', #5349 ) ;
#606 = CIRCLE ( 'NONE', #4981, 4.749999999999999112 ) ;
#607 = ORIENTED_EDGE ( 'NONE', *, *, #3154, .F. ) ;
#608 =( NAMED_UNIT ( * ) PLANE_ANGLE_UNIT ( ) SI_UNIT ( $, .RADIAN. ) );
#609 = DIRECTION ( 'NONE',  ( 1.000000000000000000, -0.000000000000000000, 0.000000000000000000 ) ) ;
#610 = ORIENTED_EDGE ( 'NONE', *, *, #5795, .F. ) ;
#611 = EDGE_CURVE ( 'NONE', #5793, #5838, #2551, .T. ) ;
#612 = MECHANICAL_DESIGN_GEOMETRIC_PRESENTATION_REPRESENTATION (  '', ( #2355 ), #5740 ) ;
#613 = CARTESIAN_POINT ( 'NONE',  ( 57.00000000000002132, -1.278008170942866441E-15, 75.00000000000000000 ) ) ;
#614 = CARTESIAN_POINT ( 'NONE',  ( -74.99999999999998579, 15.00000000000000000, -75.00000000000000000 ) ) ;
#615 = PRODUCT_DEFINITION_FORMATION_WITH_SPECIFIED_SOURCE ( 'ANY', '', #682, .NOT_KNOWN. ) ;
#616 = DIRECTION ( 'NONE',  ( 0.000000000000000000, -1.000000000000000000, -3.491481338843133355E-15 ) ) ;
#617 = ADVANCED_FACE ( 'NONE', ( #2607 ), #229, .F. ) ;
#618 = EDGE_LOOP ( 'NONE', ( #5048, #5006, #2179, #2034 ) ) ;
#619 = EDGE_LOOP ( 'NONE', ( #1180, #3918, #3535, #5634, #2377, #231, #3566, #1991 ) ) ;
#620 = SURFACE_STYLE_USAGE ( .BOTH. , #4809 ) ;
#621 = FACE_OUTER_BOUND ( 'NONE', #3054, .T. ) ;
#622 = ORIENTED_EDGE ( 'NONE', *, *, #578, .T. ) ;
#623 = FACE_OUTER_BOUND ( 'NONE', #2477, .T. ) ;
#624 = CARTESIAN_POINT ( 'NONE',  ( -45.00000000000001421, 50.00000000000000000, 50.00000000000000000 ) ) ;
#625 = DIRECTION ( 'NONE',  ( -0.000000000000000000, -1.000000000000000000, -0.000000000000000000 ) ) ;
#626 = VERTEX_POINT ( 'NONE', #3463 ) ;
#627 = DIRECTION ( 'NONE',  ( -2.081668171172168513E-17, -0.9124080317073151036, -0.4092817900615456916 ) ) ;
#628 = DIRECTION ( 'NONE',  ( -0.000000000000000000, -1.000000000000000000, -0.000000000000000000 ) ) ;
#629 = DIRECTION ( 'NONE',  ( -0.000000000000000000, -1.000000000000000000, -0.000000000000000000 ) ) ;
#630 = FACE_OUTER_BOUND ( 'NONE', #4465, .T. ) ;
#631 = FACE_OUTER_BOUND ( 'NONE', #5917, .T. ) ;
#632 = FACE_OUTER_BOUND ( 'NONE', #5560, .T. ) ;
#633 = ORIENTED_EDGE ( 'NONE', *, *, #3059, .T. ) ;
#635 = VERTEX_POINT ( 'NONE', #347 ) ;
#634 = PRODUCT_DEFINITION_SHAPE ( 'NONE', 'NONE',  #5977 ) ;
#636 = LINE ( 'NONE', #1087, #4113 ) ;
#637 = UNCERTAINTY_MEASURE_WITH_UNIT (LENGTH_MEASURE( 1.000000000000000082E-05 ), #2820, 'distance_accuracy_value', 'NONE');
#638 = ORIENTED_EDGE ( 'NONE', *, *, #2527, .F. ) ;
#639 = SURFACE_STYLE_USAGE ( .BOTH. , #1582 ) ;
#640 = EDGE_CURVE ( 'NONE', #3205, #5222, #255, .T. ) ;
#641 = LINE ( 'NONE', #2484, #4530 ) ;
#642 = EDGE_CURVE ( 'NONE', #3435, #4780, #1614, .T. ) ;
#643 = ADVANCED_FACE ( 'NONE', ( #3491, #4470 ), #669, .F. ) ;
#644 = CIRCLE ( 'NONE', #5781, 0.8509999999999999787 ) ;
#645 = DIRECTION ( 'NONE',  ( 0.000000000000000000, 0.000000000000000000, -1.000000000000000000 ) ) ;
#647 = ORIENTED_EDGE ( 'NONE', *, *, #1643, .T. ) ;
#646 = ADVANCED_FACE ( 'NONE', ( #1584 ), #3437, .T. ) ;
#648 = ORIENTED_EDGE ( 'NONE', *, *, #3065, .F. ) ;
#649 = DIRECTION ( 'NONE',  ( 0.000000000000000000, 0.000000000000000000, 1.000000000000000000 ) ) ;
#650 = ORIENTED_EDGE ( 'NONE', *, *, #39, .T. ) ;
#651 = DIRECTION ( 'NONE',  ( -0.000000000000000000, -0.000000000000000000, 1.000000000000000000 ) ) ;
#652 = CARTESIAN_POINT ( 'NONE',  ( 60.00000000000001421, -1.951563910473909559E-15, -65.00000000000000000 ) ) ;
#653 = FACE_OUTER_BOUND ( 'NONE', #742, .T. ) ;
#654 = ORIENTED_EDGE ( 'NONE', *, *, #3425, .F. ) ;
#655 = SHAPE_DEFINITION_REPRESENTATION ( #1105, #951 ) ;
#656 = EDGE_CURVE ( 'NONE', #3756, #3717, #1676, .T. ) ;
#657 = DIRECTION ( 'NONE',  ( 0.000000000000000000, 0.000000000000000000, 1.000000000000000000 ) ) ;
#658 = CARTESIAN_POINT ( 'NONE',  ( 1.314929834301322591E-16, 0.000000000000000000, 0.000000000000000000 ) ) ;
#659 = DIRECTION ( 'NONE',  ( -1.000000000000000000, -0.000000000000000000, -0.000000000000000000 ) ) ;
#660 = CARTESIAN_POINT ( 'NONE',  ( 150.0000000000000284, 15.00000000000000000, -45.00000000000000000 ) ) ;
#661 = DIRECTION ( 'NONE',  ( 1.000000000000000000, -0.000000000000000000, -0.000000000000000000 ) ) ;
#662 = ORIENTED_EDGE ( 'NONE', *, *, #2796, .F. ) ;
#663 = AXIS2_PLACEMENT_3D ( 'NONE', #4941, #4491, #775 ) ;
#664 = ORIENTED_EDGE ( 'NONE', *, *, #5133, .F. ) ;
#665 = CARTESIAN_POINT ( 'NONE',  ( 1.849560077140141257, -0.7556913915602415655, -0.5150000000000000133 ) ) ;
#666 = VERTEX_POINT ( 'NONE', #3916 ) ;
#667 = DIRECTION ( 'NONE',  ( 1.000000000000000000, 0.000000000000000000, 0.000000000000000000 ) ) ;
#668 = CIRCLE ( 'NONE', #4059, 1.336466033005844434 ) ;
#669 = PLANE ( 'NONE',  #4650 ) ;
#670 = FACE_OUTER_BOUND ( 'NONE', #1139, .T. ) ;
#671 = CIRCLE ( 'NONE', #1146, 2.000000000000000000 ) ;
#672 = EDGE_LOOP ( 'NONE', ( #2871, #913, #5493, #5863 ) ) ;
#673 = EDGE_CURVE ( 'NONE', #771, #4908, #3765, .T. ) ;
#674 = VERTEX_POINT ( 'NONE', #3042 ) ;
#675 = VECTOR ( 'NONE', #3854, 1000.000000000000000 ) ;
#676 = AXIS2_PLACEMENT_3D ( 'NONE', #3452, #3515, #5369 ) ;
#677 = EDGE_CURVE ( 'NONE', #3503, #2491, #2020, .T. ) ;
#678 = DIRECTION ( 'NONE',  ( 0.000000000000000000, 0.000000000000000000, -1.000000000000000000 ) ) ;
#679 = ORIENTED_EDGE ( 'NONE', *, *, #761, .F. ) ;
#680 = FACE_OUTER_BOUND ( 'NONE', #139, .T. ) ;
#681 = CARTESIAN_POINT ( 'NONE',  ( 62.50000000000001421, -1.951563910473909559E-15, 75.00000000000000000 ) ) ;
#682 = PRODUCT ( 'guide track', 'guide track', '', ( #3710 ) ) ;
#683 = CARTESIAN_POINT ( 'NONE',  ( 55.00000000000000711, 0.000000000000000000, 0.000000000000000000 ) ) ;
#684 = AXIS2_PLACEMENT_3D ( 'NONE', #5967, #4087, #2630 ) ;
#685 = ORIENTED_EDGE ( 'NONE', *, *, #934, .F. ) ;
#686 = APPLICATION_PROTOCOL_DEFINITION ( 'draft international standard', 'automotive_design', 1998, #4712 ) ;
#687 = DIRECTION ( 'NONE',  ( -1.000000000000000000, -0.000000000000000000, -0.000000000000000000 ) ) ;
#688 = CIRCLE ( 'NONE', #1363, 2.500000000000002220 ) ;
#689 = VECTOR ( 'NONE', #5205, 1000.000000000000000 ) ;
#690 = DIRECTION ( 'NONE',  ( -0.000000000000000000, -0.000000000000000000, 1.000000000000000000 ) ) ;
#691 = CARTESIAN_POINT ( 'NONE',  ( 2.740000000000000213, -0.5150000000000034550, 0.9838866223909985553 ) ) ;
#692 = FACE_OUTER_BOUND ( 'NONE', #2283, .T. ) ;
#693 = CARTESIAN_POINT ( 'NONE',  ( 62.50000000000001421, -1.951563910473909559E-15, 75.00000000000000000 ) ) ;
#694 = EDGE_CURVE ( 'NONE', #695, #4416, #2094, .T. ) ;
#695 = VERTEX_POINT ( 'NONE', #1702 ) ;
#696 = VECTOR ( 'NONE', #1255, 1000.000000000000000 ) ;
#697 = AXIS2_PLACEMENT_3D ( 'NONE', #1015, #2868, #3805 ) ;
#698 = VERTEX_POINT ( 'NONE', #4958 ) ;
#699 = DIRECTION ( 'NONE',  ( 1.000000000000000000, 0.000000000000000000, 0.000000000000000000 ) ) ;
#700 = PRODUCT_DEFINITION_CONTEXT ( 'detailed design', #4605, 'design' ) ;
#701 = VECTOR ( 'NONE', #83, 1000.000000000000000 ) ;
#702 = VERTEX_POINT ( 'NONE', #792 ) ;
#703 = CIRCLE ( 'NONE', #318, 7.864440107515624945 ) ;
#704 = VECTOR ( 'NONE', #489, 1000.000000000000341 ) ;
#705 = VECTOR ( 'NONE', #452, 1000.000000000000000 ) ;
#706 = CARTESIAN_POINT ( 'NONE',  ( 20.85786437626904899, 0.000000000000000000, -5.000000000000000000 ) ) ;
#707 = PLANE ( 'NONE',  #3487 ) ;
#708 = VERTEX_POINT ( 'NONE', #3229 ) ;
#709 = ORIENTED_EDGE ( 'NONE', *, *, #461, .F. ) ;
#710 =( NAMED_UNIT ( * ) PLANE_ANGLE_UNIT ( ) SI_UNIT ( $, .RADIAN. ) );
#711 = AXIS2_PLACEMENT_3D ( 'NONE', #2471, #3957, #4789 ) ;
#712 = CARTESIAN_POINT ( 'NONE',  ( 137.4999999999999716, 15.00000000000000000, -75.00000000000000000 ) ) ;
#713 = EDGE_LOOP ( 'NONE', ( #4575, #4451 ) ) ;
#714 = DIRECTION ( 'NONE',  ( 0.000000000000000000, 1.000000000000000000, 0.000000000000000000 ) ) ;
#715 = CARTESIAN_POINT ( 'NONE',  ( 75.00000000000001421, 0.000000000000000000, 0.000000000000000000 ) ) ;
#716 = CARTESIAN_POINT ( 'NONE',  ( -45.00000000000001421, 40.00000000000000000, -55.00000000000000000 ) ) ;
#717 = EDGE_LOOP ( 'NONE', ( #3429, #5530, #303, #5193 ) ) ;
#718 = APPLICATION_PROTOCOL_DEFINITION ( 'draft international standard', 'automotive_design', 1998, #4605 ) ;
#719 = EDGE_CURVE ( 'NONE', #4755, #3109, #5913, .T. ) ;
#720 = CARTESIAN_POINT ( 'NONE',  ( -45.00000000000001421, 40.00000000000000000, -45.00000000000000000 ) ) ;
#721 = ADVANCED_FACE ( 'NONE', ( #2279 ), #5554, .F. ) ;
#722 = DIRECTION ( 'NONE',  ( 0.8660254037844383745, 0.000000000000000000, -0.5000000000000004441 ) ) ;
#723 = CARTESIAN_POINT ( 'NONE',  ( 37.50000000000000711, 6.288372600415927295E-15, -65.00000000000000000 ) ) ;
#724 = DIRECTION ( 'NONE',  ( 0.000000000000000000, 1.065814103640150121E-14, 1.000000000000000000 ) ) ;
#725 = DIRECTION ( 'NONE',  ( 0.000000000000000000, -1.000000000000000000, 0.000000000000000000 ) ) ;
#726 = VERTEX_POINT ( 'NONE', #5022 ) ;
#727 = EDGE_CURVE ( 'NONE', #525, #782, #3196, .T. ) ;
#728 = ORIENTED_EDGE ( 'NONE', *, *, #2465, .F. ) ;
#729 = DIRECTION ( 'NONE',  ( -1.000000000000000000, -0.000000000000000000, -0.000000000000000000 ) ) ;
#730 = VECTOR ( 'NONE', #4229, 1000.000000000000000 ) ;
#731 = ORIENTED_EDGE ( 'NONE', *, *, #3681, .T. ) ;
#732 = CARTESIAN_POINT ( 'NONE',  ( 75.00000000000001421, -7.000000000000006217, 65.00000000000000000 ) ) ;
#733 = ADVANCED_FACE ( 'NONE', ( #10 ), #5052, .F. ) ;
#734 = DIRECTION ( 'NONE',  ( 0.5150380737757185301, 0.000000000000000000, -0.8571673013836900168 ) ) ;
#735 = EDGE_LOOP ( 'NONE', ( #5844, #4817, #4105, #4046 ) ) ;
#736 = VERTEX_POINT ( 'NONE', #4158 ) ;
#737 = FILL_AREA_STYLE ('',( #2163 ) ) ;
#738 = FILL_AREA_STYLE_COLOUR ( '', #2898 ) ;
#739 = ORIENTED_EDGE ( 'NONE', *, *, #1238, .F. ) ;
#740 = PLANE ( 'NONE',  #879 ) ;
#741 = DIRECTION ( 'NONE',  ( 1.000000000000000000, 0.000000000000000000, 0.000000000000000000 ) ) ;
#742 = EDGE_LOOP ( 'NONE', ( #3170, #5345, #1739, #1388 ) ) ;
#743 = CARTESIAN_POINT ( 'NONE',  ( 75.00000000000001421, 0.000000000000000000, -9.500000000000000000 ) ) ;
#744 = ORIENTED_EDGE ( 'NONE', *, *, #1156, .T. ) ;
#745 = CONTEXT_DEPENDENT_SHAPE_REPRESENTATION ( #5249, #4805 ) ;
#746 = CARTESIAN_POINT ( 'NONE',  ( 0.9586399445693771781, -0.5149999999999964606, -0.8293189044373090457 ) ) ;
#747 = PLANE ( 'NONE',  #3499 ) ;
#748 = DIRECTION ( 'NONE',  ( 0.000000000000000000, 0.000000000000000000, -1.000000000000000000 ) ) ;
#749 = CARTESIAN_POINT ( 'NONE',  ( 137.4999999999999716, 8.572527594031473190E-16, 7.000000000000000000 ) ) ;
#750 = CARTESIAN_POINT ( 'NONE',  ( 37.50000000000000711, 6.288372600415927295E-15, -53.49784845693390167 ) ) ;
#751 = EDGE_CURVE ( 'NONE', #4020, #342, #703, .T. ) ;
#752 = ORIENTED_EDGE ( 'NONE', *, *, #5216, .F. ) ;
#753 = EDGE_CURVE ( 'NONE', #5930, #5402, #4102, .T. ) ;
#754 = LINE ( 'NONE', #5791, #1297 ) ;
#755 = EDGE_CURVE ( 'NONE', #2883, #5520, #1571, .T. ) ;
#756 = ORIENTED_EDGE ( 'NONE', *, *, #1523, .T. ) ;
#757 = CARTESIAN_POINT ( 'NONE',  ( 1.299999999999999156, 0.000000000000000000, 0.000000000000000000 ) ) ;
#758 = FILL_AREA_STYLE ('',( #4927 ) ) ;
#759 = CARTESIAN_POINT ( 'NONE',  ( -45.00000000000001421, 15.00000000000000000, 50.00000000000000000 ) ) ;
#760 = CARTESIAN_POINT ( 'NONE',  ( 2.740000000000000213, 0.9838866223910001096, 0.5149999999999999023 ) ) ;
#761 = EDGE_CURVE ( 'NONE', #3012, #1071, #546, .T. ) ;
#762 = ORIENTED_EDGE ( 'NONE', *, *, #2902, .T. ) ;
#763 = EDGE_CURVE ( 'NONE', #2775, #5479, #5431, .T. ) ;
#764 = VERTEX_POINT ( 'NONE', #4131 ) ;
#765 = SURFACE_SIDE_STYLE ('',( #1681 ) ) ;
#766 = AXIS2_PLACEMENT_3D ( 'NONE', #2403, #4266, #2375 ) ;
#767 = DIRECTION ( 'NONE',  ( 0.000000000000000000, 0.000000000000000000, 1.000000000000000000 ) ) ;
#768 = ORIENTED_EDGE ( 'NONE', *, *, #864, .F. ) ;
#769 = CARTESIAN_POINT ( 'NONE',  ( -45.00000000000001421, 30.00000000000000355, 45.00000000000000000 ) ) ;
#770 = CARTESIAN_POINT ( 'NONE',  ( 19.70000000000000284, 3.061616997868383141E-16, -2.500000000000000000 ) ) ;
#771 = VERTEX_POINT ( 'NONE', #881 ) ;
#772 = CARTESIAN_POINT ( 'NONE',  ( 0.5000000000000000000, -0.2499999999999997780, -1.911797424705720116 ) ) ;
#773 = ORIENTED_EDGE ( 'NONE', *, *, #751, .T. ) ;
#774 = AXIS2_PLACEMENT_3D ( 'NONE', #3204, #5115, #943 ) ;
#775 = DIRECTION ( 'NONE',  ( 0.000000000000000000, 0.000000000000000000, -1.000000000000000000 ) ) ;
#776 = DIRECTION ( 'NONE',  ( 0.000000000000000000, 1.000000000000000000, 0.000000000000000000 ) ) ;
#777 = VECTOR ( 'NONE', #5468, 1000.000000000000000 ) ;
#778 = CYLINDRICAL_SURFACE ( 'NONE', #4471, 2.649999999999999467 ) ;
#779 = UNCERTAINTY_MEASURE_WITH_UNIT (LENGTH_MEASURE( 1.000000000000000082E-05 ), #1753, 'distance_accuracy_value', 'NONE');
#780 = DIRECTION ( 'NONE',  ( 1.000000000000000000, -0.000000000000000000, -0.000000000000000000 ) ) ;
#781 = CARTESIAN_POINT ( 'NONE',  ( 0.5000000000000000000, 0.000000000000000000, 1.928074011315806136 ) ) ;
#782 = VERTEX_POINT ( 'NONE', #4645 ) ;
#783 = FILL_AREA_STYLE_COLOUR ( '', #132 ) ;
#784 = CIRCLE ( 'NONE', #2623, 4.999999999999990230 ) ;
#785 = CARTESIAN_POINT ( 'NONE',  ( 2.740000000000000213, 0.6774776749089228556, 0.5149999999999997913 ) ) ;
#786 = EDGE_LOOP ( 'NONE', ( #1518, #4648, #5760, #5056 ) ) ;
#787 = CIRCLE ( 'NONE', #2331, 0.2000000000000000944 ) ;
#789 = AXIS2_PLACEMENT_3D ( 'NONE', #658, #2109, #3959 ) ;
#788 = DIRECTION ( 'NONE',  ( 0.000000000000000000, -0.000000000000000000, 1.000000000000000000 ) ) ;
#790 = APPLICATION_CONTEXT ( 'automotive_design' ) ;
#791 = PRODUCT_DEFINITION ( 'UNKNOWN', '', #4303, #1117 ) ;
#792 = CARTESIAN_POINT ( 'NONE',  ( -74.99999999999998579, -15.00000000000000000, -75.00000000000000000 ) ) ;
#793 = EDGE_CURVE ( 'NONE', #853, #1083, #1370, .T. ) ;
#794 = CARTESIAN_POINT ( 'NONE',  ( 25.00000000000000711, -6.999999999999989342, -75.00000000000000000 ) ) ;
#795 = VECTOR ( 'NONE', #780, 1000.000000000000000 ) ;
#796 = EDGE_LOOP ( 'NONE', ( #4911, #5822 ) ) ;
#797 = COLOUR_RGB ( '',0.8941176470588234615, 0.8941176470588234615, 0.8941176470588234615 ) ;
#798 = ORIENTED_EDGE ( 'NONE', *, *, #4836, .F. ) ;
#799 = SURFACE_SIDE_STYLE ('',( #3501 ) ) ;
#800 = ADVANCED_FACE ( 'NONE', ( #4623 ), #374, .T. ) ;
#801 = LINE ( 'NONE', #1707, #2409 ) ;
#802 = EDGE_LOOP ( 'NONE', ( #5147, #2545, #5941, #1768 ) ) ;
#803 = LINE ( 'NONE', #4483, #970 ) ;
#804 = CARTESIAN_POINT ( 'NONE',  ( -74.99999999999998579, -15.00000000000000000, 75.00000000000000000 ) ) ;
#805 = VERTEX_POINT ( 'NONE', #4561 ) ;
#806 = CARTESIAN_POINT ( 'NONE',  ( 0.3612935698783896754, -0.2499999999999997224, -1.888152147991466245 ) ) ;
#807 = ORIENTED_EDGE ( 'NONE', *, *, #4472, .F. ) ;
#808 = STYLED_ITEM ( 'NONE', ( #3256 ), #3558 ) ;
#809 = APPLICATION_PROTOCOL_DEFINITION ( 'draft international standard', 'automotive_design', 1998, #790 ) ;
#810 = ADVANCED_FACE ( 'NONE', ( #4064 ), #3617, .T. ) ;
#811 = CARTESIAN_POINT ( 'NONE',  ( 24.99999999999998224, -7.000000000000006217, 75.00000000000000000 ) ) ;
#812 = ORIENTED_EDGE ( 'NONE', *, *, #1765, .T. ) ;
#813 = CARTESIAN_POINT ( 'NONE',  ( -35.00000000000000711, 30.00000000000000355, 45.00000000000000000 ) ) ;
#814 = LINE ( 'NONE', #392, #319 ) ;
#815 = FACE_OUTER_BOUND ( 'NONE', #1902, .T. ) ;
#816 = ORIENTED_EDGE ( 'NONE', *, *, #562, .F. ) ;
#817 =( NAMED_UNIT ( * ) PLANE_ANGLE_UNIT ( ) SI_UNIT ( $, .RADIAN. ) );
#818 = DIRECTION ( 'NONE',  ( 1.000000000000000000, 0.000000000000000000, 0.000000000000000000 ) ) ;
#819 = ORIENTED_EDGE ( 'NONE', *, *, #5570, .T. ) ;
#820 = CARTESIAN_POINT ( 'NONE',  ( -40.66987298107780902, 45.00000000000000000, 52.49999999999999289 ) ) ;
#821 = CARTESIAN_POINT ( 'NONE',  ( 150.0000000000000284, 15.00000000000000000, 45.00000000000000000 ) ) ;
#822 = DIRECTION ( 'NONE',  ( -0.000000000000000000, -1.000000000000000000, 0.000000000000000000 ) ) ;
#823 = VERTEX_POINT ( 'NONE', #2303 ) ;
#824 = EDGE_CURVE ( 'NONE', #5481, #3560, #1471, .T. ) ;
#825 = ORIENTED_EDGE ( 'NONE', *, *, #2684, .T. ) ;
#826 = EDGE_CURVE ( 'NONE', #3782, #1794, #404, .T. ) ;
#827 = FACE_OUTER_BOUND ( 'NONE', #1704, .T. ) ;
#828 = ADVANCED_FACE ( 'NONE', ( #2247 ), #4194, .F. ) ;
#829 = FILL_AREA_STYLE_COLOUR ( '', #4265 ) ;
#830 = EDGE_LOOP ( 'NONE', ( #5101, #4107, #648, #1776 ) ) ;
#831 = ADVANCED_FACE ( 'NONE', ( #1816 ), #2821, .F. ) ;
#832 = DIRECTION ( 'NONE',  ( 0.000000000000000000, 1.000000000000000000, 0.000000000000000000 ) ) ;
#833 = CYLINDRICAL_SURFACE ( 'NONE', #3407, 5.000000000000004441 ) ;
#834 = ORIENTED_EDGE ( 'NONE', *, *, #3551, .F. ) ;
#835 = DIRECTION ( 'NONE',  ( -1.000000000000000000, 0.000000000000000000, 0.000000000000000000 ) ) ;
#836 = ORIENTED_EDGE ( 'NONE', *, *, #106, .F. ) ;
#837 = AXIS2_PLACEMENT_3D ( 'NONE', #3251, #4553, #3698 ) ;
#838 = DIRECTION ( 'NONE',  ( -1.000000000000000000, -0.000000000000000000, -0.000000000000000000 ) ) ;
#839 = CIRCLE ( 'NONE', #5777, 7.983406227920510467 ) ;
#840 = DIRECTION ( 'NONE',  ( 0.000000000000000000, 1.000000000000000000, 0.000000000000000000 ) ) ;
#841 = CARTESIAN_POINT ( 'NONE',  ( 0.2307700686259116507, -0.2500000000000000000, 1.812750528907549175 ) ) ;
#842 = DIRECTION ( 'NONE',  ( 0.000000000000000000, 0.000000000000000000, -1.000000000000000000 ) ) ;
#843 = FACE_OUTER_BOUND ( 'NONE', #2021, .T. ) ;
#844 = EDGE_LOOP ( 'NONE', ( #1420, #2357 ) ) ;
#845 = ADVANCED_FACE ( 'NONE', ( #4282 ), #4736, .F. ) ;
#846 =( NAMED_UNIT ( * ) PLANE_ANGLE_UNIT ( ) SI_UNIT ( $, .RADIAN. ) );
#847 = DIRECTION ( 'NONE',  ( 0.000000000000000000, -1.000000000000000000, 0.000000000000000000 ) ) ;
#848 = ORIENTED_EDGE ( 'NONE', *, *, #3434, .T. ) ;
#849 = LINE ( 'NONE', #1272, #3893 ) ;
#850 = CARTESIAN_POINT ( 'NONE',  ( -25.39999999999996305, 0.000000000000000000, 0.000000000000000000 ) ) ;
#851 = LINE ( 'NONE', #794, #3395 ) ;
#852 = ORIENTED_EDGE ( 'NONE', *, *, #5084, .T. ) ;
#853 = VERTEX_POINT ( 'NONE', #1421 ) ;
#854 = CARTESIAN_POINT ( 'NONE',  ( -45.00000000000001421, 40.00000000000000000, 45.00000000000000000 ) ) ;
#855 = FACE_OUTER_BOUND ( 'NONE', #329, .T. ) ;
#856 = EDGE_LOOP ( 'NONE', ( #5146, #4252 ) ) ;
#857 = CARTESIAN_POINT ( 'NONE',  ( -996.9834933385058093, 0.000000000000000000, 0.000000000000000000 ) ) ;
#858 = CARTESIAN_POINT ( 'NONE',  ( -45.00000000000001421, 40.00000000000000000, 45.00000000000000000 ) ) ;
#859 = ADVANCED_FACE ( 'NONE', ( #3753 ), #1050, .F. ) ;
#860 = ORIENTED_EDGE ( 'NONE', *, *, #461, .T. ) ;
#861 = CARTESIAN_POINT ( 'NONE',  ( 40.00000000000000711, 6.288372600415927295E-15, 65.00000000000000000 ) ) ;
#862 = ORIENTED_EDGE ( 'NONE', *, *, #5334, .T. ) ;
#863 = CARTESIAN_POINT ( 'NONE',  ( 162.5000000000000000, -15.00000000000000000, 75.00000000000001421 ) ) ;
#864 = EDGE_CURVE ( 'NONE', #1686, #2079, #5088, .T. ) ;
#865 = CIRCLE ( 'NONE', #5519, 7.000000000000000000 ) ;
#866 = DIRECTION ( 'NONE',  ( 0.000000000000000000, 1.000000000000000000, 0.000000000000000000 ) ) ;
#867 =( REPRESENTATION_RELATIONSHIP ('NONE','NONE', #5609, #3184 ) REPRESENTATION_RELATIONSHIP_WITH_TRANSFORMATION ( #490 )SHAPE_REPRESENTATION_RELATIONSHIP( ) );
#868 = CARTESIAN_POINT ( 'NONE',  ( 62.50000000000001421, -1.951563910473909559E-15, 75.00000000000000000 ) ) ;
#869 = FACE_OUTER_BOUND ( 'NONE', #5036, .T. ) ;
#870 = FACE_OUTER_BOUND ( 'NONE', #3951, .T. ) ;
#871 = CIRCLE ( 'NONE', #1922, 5.000000000000000000 ) ;
#872 = EDGE_LOOP ( 'NONE', ( #4611, #1557, #18, #812 ) ) ;
#873 = CYLINDRICAL_SURFACE ( 'NONE', #5492, 7.000000000000000000 ) ;
#874 = AXIS2_PLACEMENT_3D ( 'NONE', #5482, #501, #5564 ) ;
#875 = VECTOR ( 'NONE', #5916, 1000.000000000000114 ) ;
#876 = EDGE_CURVE ( 'NONE', #1861, #2678, #2267, .T. ) ;
#877 = ORIENTED_EDGE ( 'NONE', *, *, #1717, .F. ) ;
#878 = CARTESIAN_POINT ( 'NONE',  ( -45.00000000000001421, 50.00000000000000000, 39.99999999999999289 ) ) ;
#879 = AXIS2_PLACEMENT_3D ( 'NONE', #3952, #1560, #200 ) ;
#880 =( LENGTH_UNIT ( ) NAMED_UNIT ( * ) SI_UNIT ( .MILLI., .METRE. ) );
#881 = CARTESIAN_POINT ( 'NONE',  ( -45.00000000000001421, 30.00000000000000355, 39.99999999999999289 ) ) ;
#882 = AXIS2_PLACEMENT_3D ( 'NONE', #928, #4615, #5515 ) ;
#883 = AXIS2_PLACEMENT_3D ( 'NONE', #287, #2709, #1286 ) ;
#884 = CARTESIAN_POINT ( 'NONE',  ( -45.00000000000001421, 30.00000000000000355, 45.00000000000000000 ) ) ;
#885 = ORIENTED_EDGE ( 'NONE', *, *, #4953, .F. ) ;
#886 = ORIENTED_EDGE ( 'NONE', *, *, #4132, .T. ) ;
#887 = AXIS2_PLACEMENT_3D ( 'NONE', #3023, #3358, #3863 ) ;
#888 = VECTOR ( 'NONE', #173, 1000.000000000000000 ) ;
#889 = PLANE ( 'NONE',  #5001 ) ;
#890 = DIRECTION ( 'NONE',  ( 0.000000000000000000, 0.000000000000000000, 1.000000000000000000 ) ) ;
#891 = EDGE_LOOP ( 'NONE', ( #1245, #4583, #2532, #2172 ) ) ;
#892 = AXIS2_PLACEMENT_3D ( 'NONE', #1880, #1055, #2826 ) ;
#893 = AXIS2_PLACEMENT_3D ( 'NONE', #5598, #1393, #3728 ) ;
#894 = DIRECTION ( 'NONE',  ( -0.000000000000000000, -1.000000000000000000, -0.000000000000000000 ) ) ;
#895 = DIRECTION ( 'NONE',  ( 1.000000000000000000, -0.000000000000000000, -0.000000000000000000 ) ) ;
#896 = ORIENTED_EDGE ( 'NONE', *, *, #439, .F. ) ;
#897 = CARTESIAN_POINT ( 'NONE',  ( 0.000000000000000000, 0.2499999999999982792, -1.312875263449799323 ) ) ;
#898 = ORIENTED_EDGE ( 'NONE', *, *, #5242, .F. ) ;
#899 = DIRECTION ( 'NONE',  ( 0.000000000000000000, -1.000000000000000000, 0.000000000000000000 ) ) ;
#900 = VECTOR ( 'NONE', #3820, 1000.000000000000000 ) ;
#901 = CARTESIAN_POINT ( 'NONE',  ( 0.000000000000000000, 0.2499999999999982792, 1.312875263449799323 ) ) ;
#902 = PLANE ( 'NONE',  #3882 ) ;
#903 = CARTESIAN_POINT ( 'NONE',  ( 75.00000000000001421, 6.999999999999993783, 65.00000000000000000 ) ) ;
#904 = CARTESIAN_POINT ( 'NONE',  ( 162.4999999999999716, 7.000000000000013323, -65.00000000000000000 ) ) ;
#905 = ORIENTED_EDGE ( 'NONE', *, *, #3907, .F. ) ;
#906 = EDGE_CURVE ( 'NONE', #51, #2642, #3817, .T. ) ;
#907 = EDGE_CURVE ( 'NONE', #1750, #1825, #4990, .T. ) ;
#908 = DIRECTION ( 'NONE',  ( 0.000000000000000000, 0.000000000000000000, 1.000000000000000000 ) ) ;
#909 = PRODUCT_DEFINITION_FORMATION_WITH_SPECIFIED_SOURCE ( 'ANY', '', #5230, .NOT_KNOWN. ) ;
#910 = EDGE_CURVE ( 'NONE', #5326, #2440, #2911, .T. ) ;
#911 = CARTESIAN_POINT ( 'NONE',  ( 0.5000000000000000000, -0.2499999999999997780, -1.911797424705720116 ) ) ;
#912 = DIRECTION ( 'NONE',  ( 0.000000000000000000, 0.000000000000000000, -1.000000000000000000 ) ) ;
#913 = ORIENTED_EDGE ( 'NONE', *, *, #3587, .F. ) ;
#914 = CONICAL_SURFACE ( 'NONE', #4127, 0.9999999999999991118, 1.029744260000008405 ) ;
#915 = ADVANCED_FACE ( 'NONE', ( #1931, #4768 ), #4797, .F. ) ;
#916 = CARTESIAN_POINT ( 'NONE',  ( 20.85786437626904899, 0.000000000000000000, 0.000000000000000000 ) ) ;
#917 = SURFACE_SIDE_STYLE ('',( #3235 ) ) ;
#918 = ORIENTED_EDGE ( 'NONE', *, *, #3750, .T. ) ;
#919 = CARTESIAN_POINT ( 'NONE',  ( 62.50000000000001421, -1.951563910473909559E-15, 65.00000000000000000 ) ) ;
#920 = FACE_OUTER_BOUND ( 'NONE', #5008, .T. ) ;
#921 = EDGE_LOOP ( 'NONE', ( #4487, #2367, #4251 ) ) ;
#922 = ORIENTED_EDGE ( 'NONE', *, *, #1895, .T. ) ;
#923 = CARTESIAN_POINT ( 'NONE',  ( -45.00000000000001421, 15.00000000000000000, 45.00000000000000000 ) ) ;
#924 = DIRECTION ( 'NONE',  ( 0.000000000000000000, 0.000000000000000000, -1.000000000000000000 ) ) ;
#925 = LINE ( 'NONE', #2779, #2328 ) ;
#926 = AXIS2_PLACEMENT_3D ( 'NONE', #3342, #2851, #4711 ) ;
#927 = FACE_OUTER_BOUND ( 'NONE', #3682, .T. ) ;
#928 = CARTESIAN_POINT ( 'NONE',  ( 24.99999999999998224, 6.999999999999985789, 75.00000000000000000 ) ) ;
#929 = EDGE_LOOP ( 'NONE', ( #5175, #3265, #2543, #4407 ) ) ;
#930 = CARTESIAN_POINT ( 'NONE',  ( 195.9140739546802763, 0.000000000000000000, 0.9330303641814459148 ) ) ;
#931 = DIRECTION ( 'NONE',  ( 0.000000000000000000, 0.000000000000000000, 1.000000000000000000 ) ) ;
#932 = EDGE_CURVE ( 'NONE', #3440, #5157, #3043, .T. ) ;
#933 = DIRECTION ( 'NONE',  ( 1.000000000000000000, 0.000000000000000000, -0.000000000000000000 ) ) ;
#934 = EDGE_CURVE ( 'NONE', #3290, #107, #1539, .T. ) ;
#935 = VECTOR ( 'NONE', #5236, 1000.000000000000000 ) ;
#936 = EDGE_LOOP ( 'NONE', ( #4735, #3724 ) ) ;
#937 = CARTESIAN_POINT ( 'NONE',  ( 24.99999999999998224, 6.999999999999985789, 75.00000000000000000 ) ) ;
#938 = EDGE_CURVE ( 'NONE', #3605, #1770, #69, .T. ) ;
#939 = VERTEX_POINT ( 'NONE', #5636 ) ;
#940 = DIRECTION ( 'NONE',  ( 1.000000000000000000, -0.000000000000000000, -0.000000000000000000 ) ) ;
#941 = DIRECTION ( 'NONE',  ( 0.000000000000000000, 0.000000000000000000, -1.000000000000000000 ) ) ;
#942 = ITEM_DEFINED_TRANSFORMATION ( 'NONE', 'NONE', #2943,  #5080 ) ;
#943 = DIRECTION ( 'NONE',  ( 1.000000000000000000, 0.000000000000000000, 0.000000000000000000 ) ) ;
#944 = ORIENTED_EDGE ( 'NONE', *, *, #1714, .F. ) ;
#945 = ADVANCED_FACE ( 'NONE', ( #1482 ), #1994, .F. ) ;
#946 = DIRECTION ( 'NONE',  ( -1.000000000000000000, -0.000000000000000000, -0.000000000000000000 ) ) ;
#947 = ORIENTED_EDGE ( 'NONE', *, *, #3173, .T. ) ;
#948 = ORIENTED_EDGE ( 'NONE', *, *, #2872, .F. ) ;
#949 = CARTESIAN_POINT ( 'NONE',  ( -45.00000000000002842, 0.000000000000000000, -44.99999999999998579 ) ) ;
#950 = CARTESIAN_POINT ( 'NONE',  ( 0.3226060873438401089, 2.189154565102731098, 0.5149999999999992362 ) ) ;
#951 = SHAPE_REPRESENTATION ( 'pan head cross recess screw_iso_ISO 7045 - M5 x 16 - Z - 16N', ( #5080 ), #5845 ) ;
#952 = DIRECTION ( 'NONE',  ( 1.000000000000000000, 0.000000000000000000, 0.000000000000000000 ) ) ;
#953 = CARTESIAN_POINT ( 'NONE',  ( 55.00000000000000711, 0.000000000000000000, 0.000000000000000000 ) ) ;
#954 = DIRECTION ( 'NONE',  ( 0.000000000000000000, -2.105246936865057790E-16, 1.000000000000000000 ) ) ;
#955 = ORIENTED_EDGE ( 'NONE', *, *, #1985, .T. ) ;
#956 = MECHANICAL_DESIGN_GEOMETRIC_PRESENTATION_REPRESENTATION (  '', ( #188 ), #1645 ) ;
#957 = DIRECTION ( 'NONE',  ( 1.000000000000000000, 0.000000000000000000, 0.000000000000000000 ) ) ;
#958 = DIRECTION ( 'NONE',  ( 1.000000000000000000, 0.000000000000000000, 0.000000000000000000 ) ) ;
#959 = CIRCLE ( 'NONE', #1734, 5.000000000000004441 ) ;
#960 = PLANE ( 'NONE',  #893 ) ;
#961 =( GEOMETRIC_REPRESENTATION_CONTEXT ( 3 ) GLOBAL_UNCERTAINTY_ASSIGNED_CONTEXT ( ( #1965 ) ) GLOBAL_UNIT_ASSIGNED_CONTEXT ( ( #2755, #53, #2314 ) ) REPRESENTATION_CONTEXT ( 'NONE', 'WORKASPACE' ) );
#962 = ORIENTED_EDGE ( 'NONE', *, *, #2793, .T. ) ;
#963 = VECTOR ( 'NONE', #121, 1000.000000000000000 ) ;
#964 = CARTESIAN_POINT ( 'NONE',  ( 137.4999999999999716, 15.00000000000000000, 75.00000000000001421 ) ) ;
#965 = CIRCLE ( 'NONE', #403, 4.750000000000000000 ) ;
#966 = ORIENTED_EDGE ( 'NONE', *, *, #4593, .T. ) ;
#967 = DIRECTION ( 'NONE',  ( -0.000000000000000000, -0.000000000000000000, 1.000000000000000000 ) ) ;
#968 = CARTESIAN_POINT ( 'NONE',  ( -49.33012701892221230, 45.00000000000000000, 37.50000000000000000 ) ) ;
#969 = VECTOR ( 'NONE', #5788, 1000.000000000000000 ) ;
#970 = VECTOR ( 'NONE', #1314, 1000.000000000000000 ) ;
#971 = EDGE_CURVE ( 'NONE', #3782, #4485, #636, .T. ) ;
#972 = DIRECTION ( 'NONE',  ( 0.000000000000000000, 0.000000000000000000, 1.000000000000000000 ) ) ;
#973 = ORIENTED_EDGE ( 'NONE', *, *, #1191, .F. ) ;
#974 = DIRECTION ( 'NONE',  ( 0.000000000000000000, 0.000000000000000000, -1.000000000000000000 ) ) ;
#975 = AXIS2_PLACEMENT_3D ( 'NONE', #4360, #1103, #3898 ) ;
#977 = ORIENTED_EDGE ( 'NONE', *, *, #4586, .T. ) ;
#976 = EDGE_CURVE ( 'NONE', #626, #5459, #5968, .T. ) ;
#978 = AXIS2_PLACEMENT_3D ( 'NONE', #3629, #419, #3737 ) ;
#979 = ORIENTED_EDGE ( 'NONE', *, *, #5237, .F. ) ;
#980 =( REPRESENTATION_RELATIONSHIP ('NONE','NONE', #5609, #2785 ) REPRESENTATION_RELATIONSHIP_WITH_TRANSFORMATION ( #1200 )SHAPE_REPRESENTATION_RELATIONSHIP( ) );
#981 = PRESENTATION_STYLE_ASSIGNMENT (( #2266 ) ) ;
#982 = ADVANCED_FACE ( 'NONE', ( #4195 ), #5945, .F. ) ;
#983 = AXIS2_PLACEMENT_3D ( 'NONE', #5013, #5074, #3743 ) ;
#984=STYLED_ITEM('',(#5999),#4254);
#985 = DIRECTION ( 'NONE',  ( -0.000000000000000000, -1.000000000000000000, -0.000000000000000000 ) ) ;
#986 = CARTESIAN_POINT ( 'NONE',  ( 77.00000000000001421, 0.000000000000000000, 9.500000000000000000 ) ) ;
#987 = LINE ( 'NONE', #4700, #1564 ) ;
#988 = CARTESIAN_POINT ( 'NONE',  ( 162.5000000000000000, -15.00000000000000000, 75.00000000000001421 ) ) ;
#989 =( GEOMETRIC_REPRESENTATION_CONTEXT ( 3 ) GLOBAL_UNCERTAINTY_ASSIGNED_CONTEXT ( ( #3370 ) ) GLOBAL_UNIT_ASSIGNED_CONTEXT ( ( #3076, #3468, #4966 ) ) REPRESENTATION_CONTEXT ( 'NONE', 'WORKASPACE' ) );
#990 = ORIENTED_EDGE ( 'NONE', *, *, #3538, .T. ) ;
#991 = PRESENTATION_LAYER_ASSIGNMENT (  '', '', ( #4682 ) ) ;
#992 = CIRCLE ( 'NONE', #5547, 1.000000000000000000 ) ;
#993 = SURFACE_SIDE_STYLE ('',( #4244 ) ) ;
#994 = EDGE_CURVE ( 'NONE', #5382, #3899, #5379, .T. ) ;
#995 = FACE_OUTER_BOUND ( 'NONE', #13, .T. ) ;
#996 = DIRECTION ( 'NONE',  ( 0.000000000000000000, 0.000000000000000000, 1.000000000000000000 ) ) ;
#997 = CARTESIAN_POINT ( 'NONE',  ( -5.404070203482436163E-16, 0.2499999999999982792, 1.454823465665887605 ) ) ;
#998 = ORIENTED_EDGE ( 'NONE', *, *, #2662, .F. ) ;
#999 = ORIENTED_EDGE ( 'NONE', *, *, #5216, .T. ) ;
#1000 = ORIENTED_EDGE ( 'NONE', *, *, #2050, .F. ) ;
#1001 = SURFACE_STYLE_FILL_AREA ( #1903 ) ;
#1002 = DIRECTION ( 'NONE',  ( 1.000000000000000000, 0.000000000000000000, 0.000000000000000000 ) ) ;
#1003 = ORIENTED_EDGE ( 'NONE', *, *, #1751, .F. ) ;
#1004 = FACE_OUTER_BOUND ( 'NONE', #921, .T. ) ;
#1005 = DIRECTION ( 'NONE',  ( -1.000000000000000000, -0.000000000000000000, -0.000000000000000000 ) ) ;
#1006 = DIRECTION ( 'NONE',  ( 0.000000000000000000, 0.000000000000000000, 1.000000000000000000 ) ) ;
#1007 = DIRECTION ( 'NONE',  ( 0.000000000000000000, 0.000000000000000000, -1.000000000000000000 ) ) ;
#1008 = EDGE_CURVE ( 'NONE', #5390, #475, #3912, .T. ) ;
#1009 = EDGE_LOOP ( 'NONE', ( #3834, #3467, #2612, #4538 ) ) ;
#1010 = EDGE_CURVE ( 'NONE', #5437, #4485, #1606, .T. ) ;
#1011 = ORIENTED_EDGE ( 'NONE', *, *, #1756, .T. ) ;
#1012 = ADVANCED_FACE ( 'NONE', ( #2600 ), #5375, .T. ) ;
#1013 = DIRECTION ( 'NONE',  ( -1.000000000000000000, -0.000000000000000000, -0.000000000000000000 ) ) ;
#1014 = DIRECTION ( 'NONE',  ( 0.000000000000000000, 0.000000000000000000, -1.000000000000000000 ) ) ;
#1015 = CARTESIAN_POINT ( 'NONE',  ( 55.00000000000000711, 0.000000000000000000, 0.000000000000000000 ) ) ;
#1016 = PRODUCT_DEFINITION_SHAPE ( 'NONE', 'NONE',  #5985 ) ;
#1017 = DIRECTION ( 'NONE',  ( -0.000000000000000000, -0.000000000000000000, 1.000000000000000000 ) ) ;
#1018 = EDGE_LOOP ( 'NONE', ( #5388, #1028, #3124, #4232 ) ) ;
#1019 = CARTESIAN_POINT ( 'NONE',  ( 0.000000000000000000, 0.000000000000000000, -90.00000000000000000 ) ) ;
#1020 = DIRECTION ( 'NONE',  ( 1.000000000000000000, 0.000000000000000000, 0.000000000000000000 ) ) ;
#1021 = CARTESIAN_POINT ( 'NONE',  ( 0.9586399445693629673, -0.5150000000000024558, 0.8293189044373063812 ) ) ;
#1022 = EDGE_CURVE ( 'NONE', #3819, #5507, #5764, .T. ) ;
#1023 = CARTESIAN_POINT ( 'NONE',  ( 75.00000000000001421, 6.999999999999993783, -65.00000000000000000 ) ) ;
#1024 = ADVANCED_FACE ( 'NONE', ( #5313, #2547, #1115 ), #5854, .F. ) ;
#1025 = ORIENTED_EDGE ( 'NONE', *, *, #3057, .T. ) ;
#1026 = ORIENTED_EDGE ( 'NONE', *, *, #3647, .T. ) ;
#1027 = DIRECTION ( 'NONE',  ( 0.000000000000000000, 0.000000000000000000, -1.000000000000000000 ) ) ;
#1028 = ORIENTED_EDGE ( 'NONE', *, *, #5949, .F. ) ;
#1029 = CARTESIAN_POINT ( 'NONE',  ( 67.00000000000000000, 0.000000000000000000, -9.500000000000000000 ) ) ;
#1030 = CARTESIAN_POINT ( 'NONE',  ( 2.740000000000000213, 0.000000000000000000, 0.000000000000000000 ) ) ;
#1031 = LINE ( 'NONE', #137, #479 ) ;
#1032 = CARTESIAN_POINT ( 'NONE',  ( 60.00000000000001421, -1.645402210687070900E-15, 55.00000000000000000 ) ) ;
#1033 = VERTEX_POINT ( 'NONE', #5730 ) ;
#1034 = VERTEX_POINT ( 'NONE', #2118 ) ;
#1035 = CARTESIAN_POINT ( 'NONE',  ( 62.50000000000001421, -1.951563910473909559E-15, -55.00000000000000000 ) ) ;
#1036 = CARTESIAN_POINT ( 'NONE',  ( 1.084202172485504434E-16, 0.000000000000000000, 0.000000000000000000 ) ) ;
#1037 = VERTEX_POINT ( 'NONE', #252 ) ;
#1038 = DIRECTION ( 'NONE',  ( 0.000000000000000000, 0.000000000000000000, -1.000000000000000000 ) ) ;
#1039 = CARTESIAN_POINT ( 'NONE',  ( 67.00000000000001421, 0.000000000000000000, -7.000000000000000000 ) ) ;
#1040 = CARTESIAN_POINT ( 'NONE',  ( 0.000000000000000000, -0.5150000000000080069, 2.349999999999998312 ) ) ;
#1041 = VERTEX_POINT ( 'NONE', #3522 ) ;
#1042 = DIRECTION ( 'NONE',  ( 0.9989374069132286316, 0.000000000000000000, 0.04608749363411584338 ) ) ;
#1043 = LINE ( 'NONE', #3336, #3266 ) ;
#1044 = LINE ( 'NONE', #600, #400 ) ;
#1045 = DIRECTION ( 'NONE',  ( 0.000000000000000000, 0.000000000000000000, -1.000000000000000000 ) ) ;
#1046 = CARTESIAN_POINT ( 'NONE',  ( 25.00000000000000711, -6.999999999999988454, -65.00000000000000000 ) ) ;
#1047 = EDGE_LOOP ( 'NONE', ( #2451, #5773, #650 ) ) ;
#1048 = ORIENTED_EDGE ( 'NONE', *, *, #3427, .F. ) ;
#1049 = SHAPE_DEFINITION_REPRESENTATION ( #5749, #5609 ) ;
#1050 = CYLINDRICAL_SURFACE ( 'NONE', #336, 4.999999999999990230 ) ;
#1051 = UNCERTAINTY_MEASURE_WITH_UNIT (LENGTH_MEASURE( 1.000000000000000082E-05 ), #556, 'distance_accuracy_value', 'NONE');
#1052 = VECTOR ( 'NONE', #5862, 1000.000000000000000 ) ;
#1053 = EDGE_CURVE ( 'NONE', #1098, #3585, #3242, .T. ) ;
#1054 = AXIS2_PLACEMENT_3D ( 'NONE', #1824, #1337, #2748 ) ;
#1055 = DIRECTION ( 'NONE',  ( 0.000000000000000000, 1.000000000000000000, 0.000000000000000000 ) ) ;
#1056 = FACE_OUTER_BOUND ( 'NONE', #1413, .T. ) ;
#1057 = AXIS2_PLACEMENT_3D ( 'NONE', #1923, #4598, #1476 ) ;
#1058 = CARTESIAN_POINT ( 'NONE',  ( 0.000000000000000000, 0.5149999999999917977, 2.350000000000000089 ) ) ;
#1059 = CARTESIAN_POINT ( 'NONE',  ( -45.00000000000001421, 50.00000000000000000, 45.00000000000000000 ) ) ;
#1060 = ORIENTED_EDGE ( 'NONE', *, *, #1419, .T. ) ;
#1061 = VECTOR ( 'NONE', #3800, 1000.000000000000000 ) ;
#1062 = EDGE_LOOP ( 'NONE', ( #5876, #5322 ) ) ;
#1063 = AXIS2_PLACEMENT_3D ( 'NONE', #868, #1807, #4982 ) ;
#1064 = FACE_OUTER_BOUND ( 'NONE', #5144, .T. ) ;
#1065 = CARTESIAN_POINT ( 'NONE',  ( 0.5000000000000000000, 2.361209666477099964E-16, -1.928074011315806136 ) ) ;
#1066 = ORIENTED_EDGE ( 'NONE', *, *, #3945, .F. ) ;
#1067 = AXIS2_PLACEMENT_3D ( 'NONE', #3514, #3930, #4365 ) ;
#1068 = FACE_BOUND ( 'NONE', #4272, .T. ) ;
#1069 = DIRECTION ( 'NONE',  ( -0.000000000000000000, -0.000000000000000000, -1.000000000000000000 ) ) ;
#1070 = FACE_OUTER_BOUND ( 'NONE', #1401, .T. ) ;
#1071 = VERTEX_POINT ( 'NONE', #3002 ) ;
#1072 = VECTOR ( 'NONE', #4368, 1000.000000000000114 ) ;
#1073 = DIRECTION ( 'NONE',  ( 0.000000000000000000, -0.4092817900615457472, 0.9124080317073152147 ) ) ;
#1074 = COLOUR_RGB ( '',0.8941176470588234615, 0.8941176470588234615, 0.8941176470588234615 ) ;
#1075 = CARTESIAN_POINT ( 'NONE',  ( 77.00000000000001421, 6.123233995736766282E-16, 5.000000000000000000 ) ) ;
#1076 = PLANE ( 'NONE',  #1067 ) ;
#1077 = DIRECTION ( 'NONE',  ( -1.000000000000000000, 0.000000000000000000, 0.000000000000000000 ) ) ;
#1078 = DIRECTION ( 'NONE',  ( 0.000000000000000000, 1.000000000000000000, 0.000000000000000000 ) ) ;
#1079 = VECTOR ( 'NONE', #4669, 1000.000000000000000 ) ;
#1081 = VECTOR ( 'NONE', #2400, 1000.000000000000227 ) ;
#1080 = CARTESIAN_POINT ( 'NONE',  ( 8.000000000000000000, -4.837354856632045452E-15, 0.000000000000000000 ) ) ;
#1082 = EDGE_CURVE ( 'NONE', #1794, #2436, #4374, .T. ) ;
#1083 = VERTEX_POINT ( 'NONE', #2974 ) ;
#1084 = ADVANCED_FACE ( 'NONE', ( #4924 ), #4437, .F. ) ;
#1085 = ORIENTED_EDGE ( 'NONE', *, *, #4472, .T. ) ;
#1086 =( LENGTH_UNIT ( ) NAMED_UNIT ( * ) SI_UNIT ( .MILLI., .METRE. ) );
#1087 = CARTESIAN_POINT ( 'NONE',  ( 25.00000000000000711, 7.000000000000011546, -65.00000000000000000 ) ) ;
#1088 = MECHANICAL_DESIGN_GEOMETRIC_PRESENTATION_REPRESENTATION (  '', ( #3609 ), #4496 ) ;
#1089 = EDGE_CURVE ( 'NONE', #542, #3182, #754, .T. ) ;
#1090 = ORIENTED_EDGE ( 'NONE', *, *, #1641, .F. ) ;
#1091 = DIRECTION ( 'NONE',  ( 1.000000000000000000, -0.000000000000000000, -0.000000000000000000 ) ) ;
#1092 = ITEM_DEFINED_TRANSFORMATION ( 'NONE', 'NONE', #4688,  #5080 ) ;
#1093 = AXIS2_PLACEMENT_3D ( 'NONE', #62, #4730, #563 ) ;
#1094 = DIRECTION ( 'NONE',  ( 0.000000000000000000, 1.000000000000000000, 0.000000000000000000 ) ) ;
#1095 = CARTESIAN_POINT ( 'NONE',  ( 1.299999999999999156, 0.000000000000000000, 0.000000000000000000 ) ) ;
#1096 = ORIENTED_EDGE ( 'NONE', *, *, #4928, .T. ) ;
#1097 = EDGE_CURVE ( 'NONE', #698, #853, #5401, .T. ) ;
#1098 = VERTEX_POINT ( 'NONE', #3095 ) ;
#1099 = FILL_AREA_STYLE_COLOUR ( '', #2225 ) ;
#1100 = CARTESIAN_POINT ( 'NONE',  ( 24.99999999999998224, -6.999999999999985789, -75.00000000000000000 ) ) ;
#1101 = FACE_OUTER_BOUND ( 'NONE', #4420, .T. ) ;
#1102 = DIRECTION ( 'NONE',  ( 0.000000000000000000, -1.000000000000000000, 0.000000000000000000 ) ) ;
#1103 = DIRECTION ( 'NONE',  ( 1.007709689656716938E-16, 1.153406566473941260E-16, -1.000000000000000000 ) ) ;
#1104 = EDGE_LOOP ( 'NONE', ( #1187, #2444 ) ) ;
#1105 = PRODUCT_DEFINITION_SHAPE ( 'NONE', 'NONE',  #2280 ) ;
#1106 = PRODUCT_CONTEXT ( 'NONE', #5950, 'mechanical' ) ;
#1107 = CARTESIAN_POINT ( 'NONE',  ( 67.00000000000001421, 0.000000000000000000, 0.000000000000000000 ) ) ;
#1108 = FACE_OUTER_BOUND ( 'NONE', #117, .T. ) ;
#1109 = LINE ( 'NONE', #691, #3490 ) ;
#1110 = CARTESIAN_POINT ( 'NONE',  ( 3.900000000000000799, 3.306546357697853733E-16, -2.700000000000000178 ) ) ;
#1111 = LINE ( 'NONE', #4823, #969 ) ;
#1112 = ORIENTED_EDGE ( 'NONE', *, *, #5912, .T. ) ;
#1113 = SHAPE_REPRESENTATION ( 'clamp', ( #5080 ), #4776 ) ;
#1114 = ORIENTED_EDGE ( 'NONE', *, *, #763, .F. ) ;
#1115 = FACE_OUTER_BOUND ( 'NONE', #2487, .T. ) ;
#1116 = UNCERTAINTY_MEASURE_WITH_UNIT (LENGTH_MEASURE( 1.000000000000000082E-05 ), #1219, 'distance_accuracy_value', 'NONE');
#1117 = PRODUCT_DEFINITION_CONTEXT ( 'detailed design', #5329, 'design' ) ;
#1118 = ORIENTED_EDGE ( 'NONE', *, *, #4148, .T. ) ;
#1119 = ADVANCED_FACE ( 'NONE', ( #1670 ), #4896, .T. ) ;
#1120 = EDGE_CURVE ( 'NONE', #3568, #3307, #2068, .T. ) ;
#1121 = DIRECTION ( 'NONE',  ( -0.000000000000000000, 0.000000000000000000, -1.000000000000000000 ) ) ;
#1122 = FACE_BOUND ( 'NONE', #4862, .T. ) ;
#1123 = VERTEX_POINT ( 'NONE', #2479 ) ;
#1124 = ORIENTED_EDGE ( 'NONE', *, *, #3551, .T. ) ;
#1125 = SURFACE_SIDE_STYLE ('',( #5652 ) ) ;
#1126 = EDGE_CURVE ( 'NONE', #1974, #666, #220, .T. ) ;
#1127 = LINE ( 'NONE', #5200, #2704 ) ;
#1128 = ORIENTED_EDGE ( 'NONE', *, *, #2566, .T. ) ;
#1129 = FACE_OUTER_BOUND ( 'NONE', #127, .T. ) ;
#1130 = FACE_OUTER_BOUND ( 'NONE', #1722, .T. ) ;
#1131 = LINE ( 'NONE', #1040, #3987 ) ;
#1132 = EDGE_LOOP ( 'NONE', ( #2391, #4516, #2697, #3573 ) ) ;
#1133 = DIRECTION ( 'NONE',  ( 1.000000000000000000, 4.770489558936219510E-17, 0.000000000000000000 ) ) ;
#1134 = LINE ( 'NONE', #2938, #3781 ) ;
#1135 = CARTESIAN_POINT ( 'NONE',  ( 135.4999999999999716, 0.000000000000000000, 5.000000000000000000 ) ) ;
#1136 = CARTESIAN_POINT ( 'NONE',  ( 37.50000000000000711, 6.288372600415927295E-15, 53.49784845693390167 ) ) ;
#1137 = DIRECTION ( 'NONE',  ( -0.000000000000000000, 8.673617379884040402E-17, -1.000000000000000000 ) ) ;
#1138 = ORIENTED_EDGE ( 'NONE', *, *, #976, .T. ) ;
#1139 = EDGE_LOOP ( 'NONE', ( #5706, #5444, #4453, #2714 ) ) ;
#1140 = SURFACE_SIDE_STYLE ('',( #4859 ) ) ;
#1141 = DIRECTION ( 'NONE',  ( -1.000000000000000000, 0.000000000000000000, 0.000000000000000000 ) ) ;
#1142 = ORIENTED_EDGE ( 'NONE', *, *, #3725, .T. ) ;
#1143 = DIRECTION ( 'NONE',  ( 0.000000000000000000, -1.000000000000000000, 0.000000000000000000 ) ) ;
#1144 = LINE ( 'NONE', #4865, #1905 ) ;
#1145 = CARTESIAN_POINT ( 'NONE',  ( -45.00000000000001421, 28.00000000000000355, 45.00000000000000000 ) ) ;
#1146 = AXIS2_PLACEMENT_3D ( 'NONE', #2308, #3712, #890 ) ;
#1147 = VERTEX_POINT ( 'NONE', #4828 ) ;
#1148 = EDGE_CURVE ( 'NONE', #805, #2324, #239, .T. ) ;
#1149 = EDGE_LOOP ( 'NONE', ( #265, #5106 ) ) ;
#1150 = B_SPLINE_CURVE_WITH_KNOTS ( 'NONE', 3,
 ( #5395, #4613, #3157, #841, #450, #4579 ),
 .UNSPECIFIED., .F., .F.,
 ( 4, 2, 4 ),
 ( 0.0005861251363949650413, 0.001008091297609326094, 0.001430057458823687363 ),
 .UNSPECIFIED. ) ;
#1151 = EDGE_CURVE ( 'NONE', #2598, #2324, #5821, .T. ) ;
#1152 =( NAMED_UNIT ( * ) SI_UNIT ( $, .STERADIAN. ) SOLID_ANGLE_UNIT ( ) );
#1153 = AXIS2_PLACEMENT_3D ( 'NONE', #1244, #5435, #4903 ) ;
#1154 = DIRECTION ( 'NONE',  ( 0.000000000000000000, 1.000000000000000000, 1.153406566473941260E-16 ) ) ;
#1155 = VERTEX_POINT ( 'NONE', #4897 ) ;
#1156 = EDGE_CURVE ( 'NONE', #3272, #1472, #2207, .T. ) ;
#1157 = DIRECTION ( 'NONE',  ( 1.000000000000000000, 0.000000000000000000, 0.000000000000000000 ) ) ;
#1158 = DIRECTION ( 'NONE',  ( 0.000000000000000000, -1.000000000000000000, 0.000000000000000000 ) ) ;
#1159 = AXIS2_PLACEMENT_3D ( 'NONE', #3827, #1520, #5224 ) ;
#1160 = LINE ( 'NONE', #5752, #5538 ) ;
#1161 = CIRCLE ( 'NONE', #108, 5.000000000000004441 ) ;
#1162 = ORIENTED_EDGE ( 'NONE', *, *, #2458, .T. ) ;
#1163 = APPLICATION_PROTOCOL_DEFINITION ( 'draft international standard', 'automotive_design', 1998, #2024 ) ;
#1164 = CARTESIAN_POINT ( 'NONE',  ( 0.6000000000000000888, 0.000000000000000000, 1.336466033005844434 ) ) ;
#1165 = VECTOR ( 'NONE', #5568, 1000.000000000000000 ) ;
#1166 = AXIS2_PLACEMENT_3D ( 'NONE', #769, #1684, #327 ) ;
#1167 = DIRECTION ( 'NONE',  ( -1.000000000000000000, 0.000000000000000000, 0.000000000000000000 ) ) ;
#1168 = CARTESIAN_POINT ( 'NONE',  ( 137.4999999999999716, -6.999999999999985789, 75.00000000000001421 ) ) ;
#1169 = DIRECTION ( 'NONE',  ( 1.000000000000000000, -0.000000000000000000, -0.000000000000000000 ) ) ;
#1170 = FACE_OUTER_BOUND ( 'NONE', #618, .T. ) ;
#1171 = ORIENTED_EDGE ( 'NONE', *, *, #4399, .T. ) ;
#1172 = CIRCLE ( 'NONE', #218, 5.000000000000000000 ) ;
#1173 = AXIS2_PLACEMENT_3D ( 'NONE', #3537, #3080, #741 ) ;
#1174 = EDGE_CURVE ( 'NONE', #3739, #3914, #1198, .T. ) ;
#1175 = VERTEX_POINT ( 'NONE', #369 ) ;
#1176 =( LENGTH_UNIT ( ) NAMED_UNIT ( * ) SI_UNIT ( .MILLI., .METRE. ) );
#1177 = CARTESIAN_POINT ( 'NONE',  ( 34.85000000000000853, 6.612904002189975595E-15, 75.00000000000000000 ) ) ;
#1178 = VECTOR ( 'NONE', #4945, 1000.000000000000000 ) ;
#1179 =( GEOMETRIC_REPRESENTATION_CONTEXT ( 3 ) GLOBAL_UNCERTAINTY_ASSIGNED_CONTEXT ( ( #2880 ) ) GLOBAL_UNIT_ASSIGNED_CONTEXT ( ( #3851, #1675, #3797 ) ) REPRESENTATION_CONTEXT ( 'NONE', 'WORKASPACE' ) );
#1180 = ORIENTED_EDGE ( 'NONE', *, *, #1410, .F. ) ;
#1181 = CONICAL_SURFACE ( 'NONE', #4874, 0.9999999999999991118, 1.029744260000008405 ) ;
#1182 =( NAMED_UNIT ( * ) SI_UNIT ( $, .STERADIAN. ) SOLID_ANGLE_UNIT ( ) );
#1183 = DIRECTION ( 'NONE',  ( 0.000000000000000000, -0.000000000000000000, 1.000000000000000000 ) ) ;
#1184 = CARTESIAN_POINT ( 'NONE',  ( 0.000000000000000000, 2.350000000000000089, -0.5150000000000000133 ) ) ;
#1185 = STYLED_ITEM ( 'NONE', ( #4986 ), #3198 ) ;
#1186 = ORIENTED_EDGE ( 'NONE', *, *, #4972, .F. ) ;
#1187 = ORIENTED_EDGE ( 'NONE', *, *, #2618, .T. ) ;
#1188 = FILL_AREA_STYLE_COLOUR ( '', #4956 ) ;
#1189 = PRODUCT_DEFINITION_FORMATION_WITH_SPECIFIED_SOURCE ( 'ANY', '', #4115, .NOT_KNOWN. ) ;
#1190 =( NAMED_UNIT ( * ) SI_UNIT ( $, .STERADIAN. ) SOLID_ANGLE_UNIT ( ) );
#1191 = EDGE_CURVE ( 'NONE', #3398, #3444, #1963, .T. ) ;
#1192 = ORIENTED_EDGE ( 'NONE', *, *, #4065, .F. ) ;
#1193 = DIRECTION ( 'NONE',  ( -1.000000000000000000, 0.000000000000000000, 0.000000000000000000 ) ) ;
#1194 = DIRECTION ( 'NONE',  ( -1.000000000000000000, -0.000000000000000000, -0.000000000000000000 ) ) ;
#1195 = ADVANCED_FACE ( 'NONE', ( #5555 ), #3607, .T. ) ;
#1196 = ORIENTED_EDGE ( 'NONE', *, *, #4877, .T. ) ;
#1197 = LINE ( 'NONE', #5931, #2731 ) ;
#1198 = CIRCLE ( 'NONE', #435, 7.000000000000000000 ) ;
#1199 = ORIENTED_EDGE ( 'NONE', *, *, #2684, .F. ) ;
#1200 = ITEM_DEFINED_TRANSFORMATION ( 'NONE', 'NONE', #3241,  #5080 ) ;
#1201 = PRODUCT_RELATED_PRODUCT_CATEGORY ( 'part', '', ( #4798 ) ) ;
#1202 = LINE ( 'NONE', #2472, #3651 ) ;
#1203 = DIRECTION ( 'NONE',  ( 0.000000000000000000, 0.000000000000000000, -1.000000000000000000 ) ) ;
#1204 = DIRECTION ( 'NONE',  ( 0.000000000000000000, 1.000000000000000000, -0.000000000000000000 ) ) ;
#1205 = DIRECTION ( 'NONE',  ( 0.000000000000000000, 1.000000000000000000, 0.000000000000000000 ) ) ;
#1206 = DIRECTION ( 'NONE',  ( 1.000000000000000000, 0.000000000000000000, 0.000000000000000000 ) ) ;
#1207 = AXIS2_PLACEMENT_3D ( 'NONE', #3001, #4435, #3875 ) ;
#1208 = ORIENTED_EDGE ( 'NONE', *, *, #1360, .F. ) ;
#1209 = DIRECTION ( 'NONE',  ( 1.000000000000000000, -3.469446951953614189E-16, 0.000000000000000000 ) ) ;
#1210 = ADVANCED_FACE ( 'NONE', ( #5460 ), #914, .F. ) ;
#1211 = ORIENTED_EDGE ( 'NONE', *, *, #2167, .F. ) ;
#1212 =( LENGTH_UNIT ( ) NAMED_UNIT ( * ) SI_UNIT ( .MILLI., .METRE. ) );
#1213 = CARTESIAN_POINT ( 'NONE',  ( 0.000000000000000000, 0.000000000000000000, 0.000000000000000000 ) ) ;
#1214 = CARTESIAN_POINT ( 'NONE',  ( -45.00000000000001421, 30.00000000000000355, 45.00000000000000000 ) ) ;
#1215 = CARTESIAN_POINT ( 'NONE',  ( -55.00000000000001421, 30.00000000000000355, -45.00000000000000000 ) ) ;
#1216 = EDGE_LOOP ( 'NONE', ( #5110, #2401 ) ) ;
#1217 = EDGE_LOOP ( 'NONE', ( #4405, #5263, #1114, #1552 ) ) ;
#1218 = CIRCLE ( 'NONE', #2870, 7.000000000000000000 ) ;
#1219 =( LENGTH_UNIT ( ) NAMED_UNIT ( * ) SI_UNIT ( .MILLI., .METRE. ) );
#1220 = ORIENTED_EDGE ( 'NONE', *, *, #4887, .F. ) ;
#1221 = AXIS2_PLACEMENT_3D ( 'NONE', #2854, #550, #190 ) ;
#1222 = CARTESIAN_POINT ( 'NONE',  ( -35.00000000000000711, 40.00000000000000000, 45.00000000000000000 ) ) ;
#1223 = CARTESIAN_POINT ( 'NONE',  ( 57.00000000000002132, -1.278008170942866441E-15, 71.29999999999999716 ) ) ;
#1224 = ORIENTED_EDGE ( 'NONE', *, *, #826, .F. ) ;
#1225 = CARTESIAN_POINT ( 'NONE',  ( -74.99999999999998579, 15.00000000000000000, -75.00000000000000000 ) ) ;
#1226 = AXIS2_PLACEMENT_3D ( 'NONE', #1164, #3513, #2081 ) ;
#1227 = ORIENTED_EDGE ( 'NONE', *, *, #1696, .T. ) ;
#1228 = SHAPE_DEFINITION_REPRESENTATION ( #481, #3184 ) ;
#1229 = DIRECTION ( 'NONE',  ( -1.000000000000000000, -0.000000000000000000, -0.000000000000000000 ) ) ;
#1230 = CARTESIAN_POINT ( 'NONE',  ( -45.00000000000001421, 30.00000000000000355, -45.00000000000000000 ) ) ;
#1231 = DIRECTION ( 'NONE',  ( 0.000000000000000000, -1.734723475976808080E-16, 1.000000000000000000 ) ) ;
#1232 = ADVANCED_BREP_SHAPE_REPRESENTATION ( '', ( #4254, #5080 ), #2935 ) ;
#1233 = DIRECTION ( 'NONE',  ( -0.000000000000000000, -0.000000000000000000, 1.000000000000000000 ) ) ;
#1234 = PRODUCT_RELATED_PRODUCT_CATEGORY ( 'part', '', ( #494 ) ) ;
#1235 = DIRECTION ( 'NONE',  ( 0.000000000000000000, 0.000000000000000000, 1.000000000000000000 ) ) ;
#1236 = ORIENTED_EDGE ( 'NONE', *, *, #2953, .T. ) ;
#1237 = SURFACE_STYLE_USAGE ( .BOTH. , #1355 ) ;
#1238 = EDGE_CURVE ( 'NONE', #3109, #3549, #5477, .T. ) ;
#1239 = DIRECTION ( 'NONE',  ( 0.000000000000000000, 0.000000000000000000, -1.000000000000000000 ) ) ;
#1240 = EDGE_LOOP ( 'NONE', ( #1618, #286, #24, #1162 ) ) ;
#1241 = DIRECTION ( 'NONE',  ( 0.000000000000000000, 1.000000000000000000, 0.000000000000000000 ) ) ;
#1242 = EDGE_CURVE ( 'NONE', #4005, #1098, #4418, .T. ) ;
#1243 = CARTESIAN_POINT ( 'NONE',  ( 162.5000000000000000, 15.00000000000000000, 65.00000000000000000 ) ) ;
#1244 = CARTESIAN_POINT ( 'NONE',  ( 77.00000000000001421, 0.000000000000000000, 0.000000000000000000 ) ) ;
#1245 = ORIENTED_EDGE ( 'NONE', *, *, #316, .F. ) ;
#1246 = CIRCLE ( 'NONE', #4646, 2.500000000000002220 ) ;
#1247 = ORIENTED_EDGE ( 'NONE', *, *, #2767, .F. ) ;
#1248 = CYLINDRICAL_SURFACE ( 'NONE', #2633, 2.500000000000002220 ) ;
#1249 = MECHANICAL_DESIGN_GEOMETRIC_PRESENTATION_REPRESENTATION (  '', ( #293 ), #1840 ) ;
#1250 = CARTESIAN_POINT ( 'NONE',  ( 32.00000000000001421, 6.961928339946971399E-15, 75.00000000000000000 ) ) ;
#1251 = EDGE_LOOP ( 'NONE', ( #5497, #155, #2860, #3324 ) ) ;
#1252 = CARTESIAN_POINT ( 'NONE',  ( -45.00000000000001421, 28.00000000000000355, 45.00000000000000000 ) ) ;
#1253 = DIRECTION ( 'NONE',  ( -0.000000000000000000, -0.000000000000000000, 1.000000000000000000 ) ) ;
#1254 = ORIENTED_EDGE ( 'NONE', *, *, #2364, .F. ) ;
#1255 = DIRECTION ( 'NONE',  ( 0.000000000000000000, 0.000000000000000000, -1.000000000000000000 ) ) ;
#1256 = PRESENTATION_LAYER_ASSIGNMENT (  '', '', ( #4950 ) ) ;
#1257 = ORIENTED_EDGE ( 'NONE', *, *, #1573, .T. ) ;
#1258 = CARTESIAN_POINT ( 'NONE',  ( 37.50000000000000711, 6.288372600415927295E-15, 75.00000000000000000 ) ) ;
#1259 =( GEOMETRIC_REPRESENTATION_CONTEXT ( 3 ) GLOBAL_UNCERTAINTY_ASSIGNED_CONTEXT ( ( #2455 ) ) GLOBAL_UNIT_ASSIGNED_CONTEXT ( ( #2489, #5176, #194 ) ) REPRESENTATION_CONTEXT ( 'NONE', 'WORKASPACE' ) );
#1260 = VECTOR ( 'NONE', #1307, 1000.000000000000000 ) ;
#1261 = FACE_OUTER_BOUND ( 'NONE', #1992, .T. ) ;
#1262 = UNCERTAINTY_MEASURE_WITH_UNIT (LENGTH_MEASURE( 1.000000000000000082E-05 ), #1176, 'distance_accuracy_value', 'NONE');
#1263 = DIRECTION ( 'NONE',  ( 1.000000000000000000, -0.000000000000000000, -0.000000000000000000 ) ) ;
#1264 = DIRECTION ( 'NONE',  ( 1.000000000000000000, 0.000000000000000000, -0.000000000000000000 ) ) ;
#1265 = ORIENTED_EDGE ( 'NONE', *, *, #5682, .T. ) ;
#1266 = VECTOR ( 'NONE', #1893, 1000.000000000000000 ) ;
#1267 = AXIS2_PLACEMENT_3D ( 'NONE', #3330, #3691, #2405 ) ;
#1268 = FACE_BOUND ( 'NONE', #354, .T. ) ;
#1269 = ORIENTED_EDGE ( 'NONE', *, *, #4856, .T. ) ;
#1270 = ADVANCED_FACE ( 'NONE', ( #5518 ), #4128, .F. ) ;
#1271 = AXIS2_PLACEMENT_3D ( 'NONE', #5723, #1078, #2449 ) ;
#1273 = VECTOR ( 'NONE', #2528, 1000.000000000000000 ) ;
#1272 = CARTESIAN_POINT ( 'NONE',  ( 24.99999999999998224, 6.999999999999985789, 75.00000000000000000 ) ) ;
#1274 = ADVANCED_FACE ( 'NONE', ( #454 ), #4524, .F. ) ;
#1275 = ADVANCED_FACE ( 'NONE', ( #1268, #6, #1844 ), #3161, .F. ) ;
#1276 = FILL_AREA_STYLE ('',( #3580 ) ) ;
#1277 = DIRECTION ( 'NONE',  ( 1.000000000000000000, -0.000000000000000000, -0.000000000000000000 ) ) ;
#1278 = AXIS2_PLACEMENT_3D ( 'NONE', #5592, #2758, #4614 ) ;
#1279 = ADVANCED_FACE ( 'NONE', ( #2668 ), #4230, .F. ) ;
#1280 = CONICAL_SURFACE ( 'NONE', #2146, 0.9999999999999991118, 1.029744260000008405 ) ;
#1281 = DIRECTION ( 'NONE',  ( -0.000000000000000000, -1.000000000000000000, 0.000000000000000000 ) ) ;
#1282 = ORIENTED_EDGE ( 'NONE', *, *, #2699, .F. ) ;
#1283 = EDGE_LOOP ( 'NONE', ( #2205, #3350 ) ) ;
#1284 = LINE ( 'NONE', #4387, #1450 ) ;
#1285 = ORIENTED_EDGE ( 'NONE', *, *, #1568, .F. ) ;
#1286 = DIRECTION ( 'NONE',  ( 0.000000000000000000, 0.000000000000000000, 1.000000000000000000 ) ) ;
#1287 = EDGE_CURVE ( 'NONE', #2495, #4600, #3639, .T. ) ;
#1288 = DIRECTION ( 'NONE',  ( 0.000000000000000000, -1.000000000000000000, 0.000000000000000000 ) ) ;
#1289 = VERTEX_POINT ( 'NONE', #5943 ) ;
#1290 = DIRECTION ( 'NONE',  ( 1.000000000000000000, 0.000000000000000000, 0.000000000000000000 ) ) ;
#1291 = ORIENTED_EDGE ( 'NONE', *, *, #2604, .F. ) ;
#1292 = AXIS2_PLACEMENT_3D ( 'NONE', #266, #207, #1042 ) ;
#1293 = FACE_OUTER_BOUND ( 'NONE', #440, .T. ) ;
#1294 = CARTESIAN_POINT ( 'NONE',  ( 7.345657149124340535, -9.419606183588304946E-15, 1.312408941150045472 ) ) ;
#1295 =( REPRESENTATION_RELATIONSHIP ('NONE','NONE', #5609, #3184 ) REPRESENTATION_RELATIONSHIP_WITH_TRANSFORMATION ( #4978 )SHAPE_REPRESENTATION_RELATIONSHIP( ) );
#1296 = DIRECTION ( 'NONE',  ( -0.000000000000000000, -0.000000000000000000, 1.000000000000000000 ) ) ;
#1297 = VECTOR ( 'NONE', #2575, 1000.000000000000000 ) ;
#1298 = DIRECTION ( 'NONE',  ( -0.000000000000000000, -1.000000000000000000, -0.000000000000000000 ) ) ;
#1299 = FACE_OUTER_BOUND ( 'NONE', #2214, .T. ) ;
#1300 = ORIENTED_EDGE ( 'NONE', *, *, #2092, .T. ) ;
#1301 = CARTESIAN_POINT ( 'NONE',  ( -45.00000000000001421, 40.00000000000000000, 45.00000000000000000 ) ) ;
#1302 = ORIENTED_EDGE ( 'NONE', *, *, #1688, .F. ) ;
#1303 = CLOSED_SHELL ( 'NONE', ( #2062, #3732, #3754, #2960, #5833, #1769, #5035, #91, #1932, #4770, #733, #2348, #5038, #5880, #1455, #20 ) ) ;
#1304 = LINE ( 'NONE', #4061, #2536 ) ;
#1305 = CARTESIAN_POINT ( 'NONE',  ( 135.4999999999999716, 0.000000000000000000, 0.000000000000000000 ) ) ;
#1306 = EDGE_CURVE ( 'NONE', #1563, #4461, #5399, .T. ) ;
#1307 = DIRECTION ( 'NONE',  ( -0.4999999999999987232, 0.000000000000000000, 0.8660254037844393737 ) ) ;
#1309 = ORIENTED_EDGE ( 'NONE', *, *, #3862, .T. ) ;
#1308 = EDGE_CURVE ( 'NONE', #5283, #805, #3833, .T. ) ;
#1310 = ORIENTED_EDGE ( 'NONE', *, *, #5372, .T. ) ;
#1311 = FACE_OUTER_BOUND ( 'NONE', #1979, .T. ) ;
#1312 = CARTESIAN_POINT ( 'NONE',  ( 0.000000000000000000, -0.5149999999999909095, -2.350000000000000977 ) ) ;
#1313 = ORIENTED_EDGE ( 'NONE', *, *, #5182, .F. ) ;
#1314 = DIRECTION ( 'NONE',  ( 0.000000000000000000, 1.000000000000000000, 0.000000000000000000 ) ) ;
#1315 = CARTESIAN_POINT ( 'NONE',  ( 2.740000000000000213, -0.6774776749089230776, 0.5149999999999995692 ) ) ;
#1316 = ORIENTED_EDGE ( 'NONE', *, *, #4317, .F. ) ;
#1317 = LINE ( 'NONE', #4517, #118 ) ;
#1318 = ORIENTED_EDGE ( 'NONE', *, *, #3090, .T. ) ;
#1319 = PLANE ( 'NONE',  #3869 ) ;
#1320 = ADVANCED_FACE ( 'NONE', ( #5046 ), #873, .T. ) ;
#1321 = DIRECTION ( 'NONE',  ( -1.000000000000000000, 4.770489558936220126E-17, 0.000000000000000000 ) ) ;
#1322 = LINE ( 'NONE', #3635, #1361 ) ;
#1323 = LINE ( 'NONE', #3088, #3995 ) ;
#1324 = CARTESIAN_POINT ( 'NONE',  ( 0.06760930072668806801, -4.837354856632045452E-15, 0.000000000000000000 ) ) ;
#1325 = VERTEX_POINT ( 'NONE', #343 ) ;
#1326 = CARTESIAN_POINT ( 'NONE',  ( 8.000000000000000000, -0.5149999999999999023, -1.857513327677604022E-15 ) ) ;
#1327 = VERTEX_POINT ( 'NONE', #478 ) ;
#1328 = LINE ( 'NONE', #3553, #3131 ) ;
#1329 = SURFACE_STYLE_USAGE ( .BOTH. , #4559 ) ;
#1330 = AXIS2_PLACEMENT_3D ( 'NONE', #3944, #3554, #5404 ) ;
#1331 = DIRECTION ( 'NONE',  ( 0.000000000000000000, 0.000000000000000000, -1.000000000000000000 ) ) ;
#1332 = CARTESIAN_POINT ( 'NONE',  ( 172.5000000000000284, 0.000000000000000000, 5.000000000000000000 ) ) ;
#1333 = ORIENTED_EDGE ( 'NONE', *, *, #547, .T. ) ;
#1334 = VERTEX_POINT ( 'NONE', #36 ) ;
#1335 = DIRECTION ( 'NONE',  ( 0.5000000000000004441, 0.000000000000000000, 0.8660254037844383745 ) ) ;
#1336 = CIRCLE ( 'NONE', #2114, 7.864440107515430434 ) ;
#1337 = DIRECTION ( 'NONE',  ( -0.000000000000000000, -0.000000000000000000, 1.000000000000000000 ) ) ;
#1338 = ORIENTED_EDGE ( 'NONE', *, *, #3975, .F. ) ;
#1339 = CYLINDRICAL_SURFACE ( 'NONE', #4764, 5.000000000000004441 ) ;
#1340 = CARTESIAN_POINT ( 'NONE',  ( 67.00000000000000000, 0.000000000000000000, 9.500000000000000000 ) ) ;
#1341 = ADVANCED_FACE ( 'NONE', ( #2873, #5209, #120 ), #1898, .T. ) ;
#1342 = ORIENTED_EDGE ( 'NONE', *, *, #1008, .T. ) ;
#1343 = DIRECTION ( 'NONE',  ( -0.8571673013836870192, 0.000000000000000000, -0.5150380737757234151 ) ) ;
#1344 = EDGE_CURVE ( 'NONE', #5222, #2390, #1218, .T. ) ;
#1345 = VERTEX_POINT ( 'NONE', #3727 ) ;
#1346 = DIRECTION ( 'NONE',  ( 0.000000000000000000, 0.000000000000000000, -1.000000000000000000 ) ) ;
#1347 = AXIS2_PLACEMENT_3D ( 'NONE', #2165, #353, #4567 ) ;
#1348 = EDGE_CURVE ( 'NONE', #5607, #2228, #2969, .T. ) ;
#1349 = DIRECTION ( 'NONE',  ( 0.000000000000000000, 1.000000000000000000, 0.000000000000000000 ) ) ;
#1350 = LINE ( 'NONE', #425, #3589 ) ;
#1351 = CYLINDRICAL_SURFACE ( 'NONE', #1278, 1.099999999999998535 ) ;
#1352 = DIRECTION ( 'NONE',  ( 1.000000000000000000, 0.000000000000000000, 0.000000000000000000 ) ) ;
#1353 = CIRCLE ( 'NONE', #4747, 4.556291390728477886 ) ;
#1354 = ORIENTED_EDGE ( 'NONE', *, *, #3614, .F. ) ;
#1355 = SURFACE_SIDE_STYLE ('',( #5644 ) ) ;
#1356 = CARTESIAN_POINT ( 'NONE',  ( 62.50000000000001421, -1.951563910473909559E-15, 71.29999999999999716 ) ) ;
#1357 = VECTOR ( 'NONE', #5280, 1000.000000000000000 ) ;
#1358 = ORIENTED_EDGE ( 'NONE', *, *, #203, .T. ) ;
#1359 = PLANE ( 'NONE',  #4979 ) ;
#1360 = EDGE_CURVE ( 'NONE', #1588, #1770, #5159, .T. ) ;
#1361 = VECTOR ( 'NONE', #5485, 1000.000000000000000 ) ;
#1362 = DIRECTION ( 'NONE',  ( -0.000000000000000000, -0.000000000000000000, 1.000000000000000000 ) ) ;
#1363 = AXIS2_PLACEMENT_3D ( 'NONE', #4854, #3962, #2998 ) ;
#1364 = AXIS2_PLACEMENT_3D ( 'NONE', #919, #445, #1375 ) ;
#1365 = ORIENTED_EDGE ( 'NONE', *, *, #5237, .T. ) ;
#1366 = ORIENTED_EDGE ( 'NONE', *, *, #1089, .T. ) ;
#1367 = AXIS2_PLACEMENT_3D ( 'NONE', #2010, #5780, #3474 ) ;
#1368 = AXIS2_PLACEMENT_3D ( 'NONE', #858, #3655, #4231 ) ;
#1369 = CARTESIAN_POINT ( 'NONE',  ( -74.99999999999998579, -15.00000000000000000, -75.00000000000000000 ) ) ;
#1370 = CIRCLE ( 'NONE', #3703, 1.099999999999998535 ) ;
#1371 = FACE_BOUND ( 'NONE', #2481, .T. ) ;
#1372 = ORIENTED_EDGE ( 'NONE', *, *, #3013, .F. ) ;
#1373 = AXIS2_PLACEMENT_3D ( 'NONE', #3790, #1996, #2915 ) ;
#1374 = AXIS2_PLACEMENT_3D ( 'NONE', #1059, #3321, #5173 ) ;
#1375 = DIRECTION ( 'NONE',  ( 1.000000000000000000, 0.000000000000000000, 0.000000000000000000 ) ) ;
#1376 = DIRECTION ( 'NONE',  ( -1.000000000000000000, -0.000000000000000000, -0.000000000000000000 ) ) ;
#1377 = EDGE_LOOP ( 'NONE', ( #2986, #2188, #5509, #3049 ) ) ;
#1378 = ORIENTED_EDGE ( 'NONE', *, *, #3145, .F. ) ;
#1379 = DIRECTION ( 'NONE',  ( 0.000000000000000000, 0.000000000000000000, 1.000000000000000000 ) ) ;
#1380 = VECTOR ( 'NONE', #2853, 1000.000000000000000 ) ;
#1381 = ADVANCED_FACE ( 'NONE', ( #564 ), #3747, .T. ) ;
#1382 = LINE ( 'NONE', #1914, #4159 ) ;
#1383 = EDGE_CURVE ( 'NONE', #1757, #3457, #5628, .T. ) ;
#1384 = CYLINDRICAL_SURFACE ( 'NONE', #3216, 5.000000000000004441 ) ;
#1385 = LINE ( 'NONE', #5099, #5546 ) ;
#1386 = STYLED_ITEM ( 'NONE', ( #4673 ), #5436 ) ;
#1387 = PLANE ( 'NONE',  #882 ) ;
#1388 = ORIENTED_EDGE ( 'NONE', *, *, #793, .T. ) ;
#1389 = EDGE_CURVE ( 'NONE', #525, #4209, #1870, .T. ) ;
#1390 = DIRECTION ( 'NONE',  ( 0.000000000000000000, 0.000000000000000000, 1.000000000000000000 ) ) ;
#1391 = CARTESIAN_POINT ( 'NONE',  ( 1.424271237134740131, 0.000000000000000000, 0.000000000000000000 ) ) ;
#1392 = AXIS2_PLACEMENT_3D ( 'NONE', #1019, #536, #1474 ) ;
#1393 = DIRECTION ( 'NONE',  ( 4.770489558936220126E-17, -1.000000000000000000, 0.000000000000000000 ) ) ;
#1394 = ORIENTED_EDGE ( 'NONE', *, *, #5599, .F. ) ;
#1395 = DIRECTION ( 'NONE',  ( 0.4461977533473793778, -2.936240938438015166E-15, 0.8949343913984707521 ) ) ;
#1396 = ADVANCED_FACE ( 'NONE', ( #3274, #4676 ), #4731, .F. ) ;
#1397 = ORIENTED_EDGE ( 'NONE', *, *, #2208, .T. ) ;
#1398 = DIRECTION ( 'NONE',  ( 0.000000000000000000, 0.000000000000000000, -1.000000000000000000 ) ) ;
#1399 = PRODUCT ( 'plunger rod', 'plunger rod', '', ( #3836 ) ) ;
#1400 = DIRECTION ( 'NONE',  ( 0.000000000000000000, 0.000000000000000000, -1.000000000000000000 ) ) ;
#1401 = EDGE_LOOP ( 'NONE', ( #5118, #133, #685, #2620 ) ) ;
#1402 = CYLINDRICAL_SURFACE ( 'NONE', #4867, 5.000000000000000000 ) ;
#1403 = VERTEX_POINT ( 'NONE', #4704 ) ;
#1404 = ORIENTED_EDGE ( 'NONE', *, *, #565, .F. ) ;
#1405 = AXIS2_PLACEMENT_3D ( 'NONE', #101, #1936, #2917 ) ;
#1406 = FACE_OUTER_BOUND ( 'NONE', #2930, .T. ) ;
#1407 = PLANE ( 'NONE',  #766 ) ;
#1408 = DIRECTION ( 'NONE',  ( 0.000000000000000000, 0.000000000000000000, -1.000000000000000000 ) ) ;
#1409 = CARTESIAN_POINT ( 'NONE',  ( 2.740000000000000213, 0.9838866223910003317, 0.5149999999999999023 ) ) ;
#1410 = EDGE_CURVE ( 'NONE', #5520, #2063, #5108, .T. ) ;
#1411 = CARTESIAN_POINT ( 'NONE',  ( -45.00000000000001421, 40.00000000000000000, 50.00000000000000000 ) ) ;
#1412 = CIRCLE ( 'NONE', #2382, 0.8509999999999999787 ) ;
#1413 = EDGE_LOOP ( 'NONE', ( #5214, #4830, #4305 ) ) ;
#1414 = CARTESIAN_POINT ( 'NONE',  ( 0.000000000000000000, 0.000000000000000000, 0.000000000000000000 ) ) ;
#1415 = CARTESIAN_POINT ( 'NONE',  ( 60.00000000000001421, -1.645402210687070900E-15, 55.00000000000000000 ) ) ;
#1416 = CIRCLE ( 'NONE', #4234, 2.500000000000000000 ) ;
#1417 = DIRECTION ( 'NONE',  ( -1.000000000000000000, -0.000000000000000000, -0.000000000000000000 ) ) ;
#1418 = CIRCLE ( 'NONE', #2117, 10.00000000000000178 ) ;
#1419 = EDGE_CURVE ( 'NONE', #4278, #199, #2544, .T. ) ;
#1420 = ORIENTED_EDGE ( 'NONE', *, *, #4411, .F. ) ;
#1421 = CARTESIAN_POINT ( 'NONE',  ( 77.00000000000001421, 0.000000000000000000, -10.59999999999999787 ) ) ;
#1422 = ADVANCED_FACE ( 'NONE', ( #995 ), #3810, .F. ) ;
#1423 = ORIENTED_EDGE ( 'NONE', *, *, #5137, .F. ) ;
#1424 = CARTESIAN_POINT ( 'NONE',  ( -45.00000000000001421, 28.00000000000000355, 52.50000000000000000 ) ) ;
#1425 = CARTESIAN_POINT ( 'NONE',  ( -45.00000000000001421, 40.00000000000000000, -45.00000000000000000 ) ) ;
#1426 = VERTEX_POINT ( 'NONE', #5184 ) ;
#1427 = DIRECTION ( 'NONE',  ( 0.000000000000000000, 1.000000000000000000, 0.000000000000000000 ) ) ;
#1428 = ORIENTED_EDGE ( 'NONE', *, *, #1448, .T. ) ;
#1429 = ADVANCED_FACE ( 'NONE', ( #2386 ), #1532, .T. ) ;
#1430 = EDGE_LOOP ( 'NONE', ( #886, #1975, #2983, #4894 ) ) ;
#1431 = CARTESIAN_POINT ( 'NONE',  ( 3.700000000000000178, 0.000000000000000000, 0.000000000000000000 ) ) ;
#1432 = LINE ( 'NONE', #5620, #2999 ) ;
#1433 = CARTESIAN_POINT ( 'NONE',  ( 62.50000000000001421, -1.951563910473909559E-15, 65.00000000000000000 ) ) ;
#1434 = SPHERICAL_SURFACE ( 'NONE', #3606, 8.000000000000000000 ) ;
#1435 = LINE ( 'NONE', #988, #1937 ) ;
#1436 = VERTEX_POINT ( 'NONE', #3775 ) ;
#1437 = AXIS2_PLACEMENT_3D ( 'NONE', #3828, #3856, #1154 ) ;
#1438 = CARTESIAN_POINT ( 'NONE',  ( 0.000000000000000000, 0.000000000000000000, 0.000000000000000000 ) ) ;
#1439 = CARTESIAN_POINT ( 'NONE',  ( 2.740000000000000213, 0.5150000000000024558, -0.6774776749089207462 ) ) ;
#1440 = CIRCLE ( 'NONE', #5606, 2.500000000000002220 ) ;
#1441 = DIRECTION ( 'NONE',  ( -1.000000000000000000, 0.000000000000000000, 0.000000000000000000 ) ) ;
#1442 = CARTESIAN_POINT ( 'NONE',  ( 0.2309188673393134938, 0.2499999999999982792, 1.812888087824517713 ) ) ;
#1443 = VECTOR ( 'NONE', #2926, 1000.000000000000000 ) ;
#1445 = ORIENTED_EDGE ( 'NONE', *, *, #640, .T. ) ;
#1444 = PRODUCT_DEFINITION_SHAPE ( 'NONE', 'NONE',  #5976 ) ;
#1446 = AXIS2_PLACEMENT_3D ( 'NONE', #3748, #3337, #5692 ) ;
#1447 = CARTESIAN_POINT ( 'NONE',  ( 75.00000000000001421, 0.000000000000000000, 9.500000000000000000 ) ) ;
#1448 = EDGE_CURVE ( 'NONE', #1034, #4985, #1043, .T. ) ;
#1449 = EDGE_CURVE ( 'NONE', #2799, #1334, #1412, .T. ) ;
#1450 = VECTOR ( 'NONE', #3143, 1000.000000000000000 ) ;
#1451 = EDGE_CURVE ( 'NONE', #3980, #5855, #3167, .T. ) ;
#1452 = AXIS2_PLACEMENT_3D ( 'NONE', #2467, #3052, #4841 ) ;
#1453 = EDGE_LOOP ( 'NONE', ( #836, #4145 ) ) ;
#1454 = CARTESIAN_POINT ( 'NONE',  ( 150.0000000000000284, 0.000000000000000000, 40.00000000000000711 ) ) ;
#1455 = ADVANCED_FACE ( 'NONE', ( #242, #1597 ), #4455, .F. ) ;
#1456 = CARTESIAN_POINT ( 'NONE',  ( 2.740000000000000213, 0.000000000000000000, 0.000000000000000000 ) ) ;
#1457 = AXIS2_PLACEMENT_3D ( 'NONE', #3063, #4921, #5397 ) ;
#1458 = VECTOR ( 'NONE', #690, 1000.000000000000000 ) ;
#1459 = CARTESIAN_POINT ( 'NONE',  ( 35.00000000000000000, 6.288372600415927295E-15, -55.00000000000000000 ) ) ;
#1460 = VECTOR ( 'NONE', #4573, 1000.000000000000000 ) ;
#1461 = VERTEX_POINT ( 'NONE', #178 ) ;
#1462 = AXIS2_PLACEMENT_3D ( 'NONE', #2561, #4973, #4484 ) ;
#1463 = ORIENTED_EDGE ( 'NONE', *, *, #5150, .F. ) ;
#1464 = CIRCLE ( 'NONE', #416, 2.500000000000002220 ) ;
#1465 = EDGE_CURVE ( 'NONE', #5831, #1830, #5114, .T. ) ;
#1466 = DIRECTION ( 'NONE',  ( 1.000000000000000000, -3.469446951953614189E-16, -0.000000000000000000 ) ) ;
#1467 = ORIENTED_EDGE ( 'NONE', *, *, #176, .F. ) ;
#1468 = CARTESIAN_POINT ( 'NONE',  ( -45.00000000000001421, 0.000000000000000000, 45.00000000000000000 ) ) ;
#1469 = CARTESIAN_POINT ( 'NONE',  ( 135.4999999999999716, 0.000000000000000000, 0.000000000000000000 ) ) ;
#1470 = FACE_OUTER_BOUND ( 'NONE', #49, .T. ) ;
#1471 = CIRCLE ( 'NONE', #4873, 2.500000000000002220 ) ;
#1472 = VERTEX_POINT ( 'NONE', #5278 ) ;
#1473 = AXIS2_PLACEMENT_3D ( 'NONE', #5671, #1547, #5639 ) ;
#1474 = DIRECTION ( 'NONE',  ( 1.000000000000000000, 0.000000000000000000, 0.000000000000000000 ) ) ;
#1475 = CARTESIAN_POINT ( 'NONE',  ( -25.39999999999996305, 0.000000000000000000, 1.000000000000000000 ) ) ;
#1476 = DIRECTION ( 'NONE',  ( 0.000000000000000000, 0.000000000000000000, -1.000000000000000000 ) ) ;
#1477 = DIRECTION ( 'NONE',  ( 1.000000000000000000, 0.000000000000000000, 0.000000000000000000 ) ) ;
#1478 = VERTEX_POINT ( 'NONE', #295 ) ;
#1479 = DIRECTION ( 'NONE',  ( 1.000000000000000000, 0.000000000000000000, 0.000000000000000000 ) ) ;
#1480 = VERTEX_POINT ( 'NONE', #2537 ) ;
#1481 =( NAMED_UNIT ( * ) PLANE_ANGLE_UNIT ( ) SI_UNIT ( $, .RADIAN. ) );
#1482 = FACE_OUTER_BOUND ( 'NONE', #3024, .T. ) ;
#1483 = UNCERTAINTY_MEASURE_WITH_UNIT (LENGTH_MEASURE( 1.000000000000000082E-05 ), #2789, 'distance_accuracy_value', 'NONE');
#1484 = APPLICATION_CONTEXT ( 'automotive_design' ) ;
#1485 = AXIS2_PLACEMENT_3D ( 'NONE', #2148, #729, #275 ) ;
#1486 = ORIENTED_EDGE ( 'NONE', *, *, #5242, .T. ) ;
#1487 = CARTESIAN_POINT ( 'NONE',  ( 77.00000000000001421, 0.000000000000000000, 8.400000000000000355 ) ) ;
#1488 = DIRECTION ( 'NONE',  ( 0.000000000000000000, 1.000000000000000000, 0.000000000000000000 ) ) ;
#1489 = CONTEXT_DEPENDENT_SHAPE_REPRESENTATION ( #2412, #4709 ) ;
#1490 = EDGE_CURVE ( 'NONE', #2057, #2341, #3386, .T. ) ;
#1491 = CARTESIAN_POINT ( 'NONE',  ( 77.00000000000001421, 0.000000000000000000, 0.000000000000000000 ) ) ;
#1492 = CLOSED_SHELL ( 'NONE', ( #3520, #828, #4166, #800, #1012, #5772, #4546, #4729, #1195, #2843, #1970, #4319, #2376, #1795, #2420, #244, #277, #4691, #5466, #5573, #5676, #3866, #3096, #3469, #4619, #349, #359, #1907, #5471, #1274, #5504, #1279, #5853, #982 ) ) ;
#1493 = ORIENTED_EDGE ( 'NONE', *, *, #1238, .T. ) ;
#1494 = ORIENTED_EDGE ( 'NONE', *, *, #3953, .T. ) ;
#1495 = AXIS2_PLACEMENT_3D ( 'NONE', #1301, #2761, #908 ) ;
#1496 = CARTESIAN_POINT ( 'NONE',  ( 77.00000000000001421, 1.347111479062087271E-16, 10.59999999999999787 ) ) ;
#1497 = ORIENTED_EDGE ( 'NONE', *, *, #5150, .T. ) ;
#1498 = CARTESIAN_POINT ( 'NONE',  ( 55.00000000000000711, 8.572527594031473190E-16, 7.000000000000000000 ) ) ;
#1499 = FACE_OUTER_BOUND ( 'NONE', #4988, .T. ) ;
#1500 = PRODUCT_DEFINITION_SHAPE ( 'NONE', 'NONE',  #3383 ) ;
#1501 = CARTESIAN_POINT ( 'NONE',  ( -45.00000000000002842, 0.000000000000000000, -44.99999999999998579 ) ) ;
#1502 = ORIENTED_EDGE ( 'NONE', *, *, #4106, .F. ) ;
#1503 = EDGE_CURVE ( 'NONE', #5450, #5793, #209, .T. ) ;
#1504 = SURFACE_STYLE_USAGE ( .BOTH. , #993 ) ;
#1505 = CARTESIAN_POINT ( 'NONE',  ( 1.849560077140107284, 0.5150000000000026779, -0.7556913915602427867 ) ) ;
#1506 = CARTESIAN_POINT ( 'NONE',  ( 24.99999999999998224, -7.000000000000006217, 75.00000000000000000 ) ) ;
#1507 = DIRECTION ( 'NONE',  ( 0.000000000000000000, -1.000000000000000000, 0.000000000000000000 ) ) ;
#1508 = LINE ( 'NONE', #3365, #3512 ) ;
#1509 = EDGE_LOOP ( 'NONE', ( #4744, #2585 ) ) ;
#1510 = ORIENTED_EDGE ( 'NONE', *, *, #2364, .T. ) ;
#1511 = AXIS2_PLACEMENT_3D ( 'NONE', #510, #2360, #5596 ) ;
#1512 = DIRECTION ( 'NONE',  ( 0.000000000000000000, 0.000000000000000000, 1.000000000000000000 ) ) ;
#1513 = AXIS2_PLACEMENT_3D ( 'NONE', #3028, #3450, #1629 ) ;
#1514 = FACE_OUTER_BOUND ( 'NONE', #99, .T. ) ;
#1515 = CARTESIAN_POINT ( 'NONE',  ( 162.4999999999999716, -6.999999999999985789, -65.00000000000000000 ) ) ;
#1516 = CARTESIAN_POINT ( 'NONE',  ( -40.66987298107781612, 40.00000000000000000, 37.50000000000000000 ) ) ;
#1517 = B_SPLINE_CURVE_WITH_KNOTS ( 'NONE', 3,
 ( #4916, #746, #2993, #4849 ),
 .UNSPECIFIED., .F., .F.,
 ( 4, 4 ),
 ( 0.001586480563516617188, 0.004268227385920363680 ),
 .UNSPECIFIED. ) ;
#1518 = ORIENTED_EDGE ( 'NONE', *, *, #5400, .T. ) ;
#1519 = ORIENTED_EDGE ( 'NONE', *, *, #2239, .T. ) ;
#1520 = DIRECTION ( 'NONE',  ( 0.000000000000000000, 1.000000000000000000, 0.000000000000000000 ) ) ;
#1521 = CIRCLE ( 'NONE', #185, 5.499999999999991118 ) ;
#1522 = DIRECTION ( 'NONE',  ( 1.000000000000000000, 0.000000000000000000, 0.000000000000000000 ) ) ;
#1523 = EDGE_CURVE ( 'NONE', #1679, #4905, #2497, .T. ) ;
#1524 = VERTEX_POINT ( 'NONE', #1075 ) ;
#1525 = DIRECTION ( 'NONE',  ( 1.000000000000000000, 0.000000000000000000, 0.000000000000000000 ) ) ;
#1526 = EDGE_CURVE ( 'NONE', #2883, #4824, #2387, .T. ) ;
#1527 = CARTESIAN_POINT ( 'NONE',  ( 35.00000000000000000, 6.594534300202765954E-15, 65.00000000000000000 ) ) ;
#1528 = DIRECTION ( 'NONE',  ( 0.000000000000000000, -1.000000000000000000, 0.000000000000000000 ) ) ;
#1529 = ORIENTED_EDGE ( 'NONE', *, *, #4214, .F. ) ;
#1530 = CARTESIAN_POINT ( 'NONE',  ( 194.0669696358185945, 0.000000000000000000, -90.91407395468023367 ) ) ;
#1531 = ADVANCED_FACE ( 'NONE', ( #4888 ), #4790, .F. ) ;
#1532 = CYLINDRICAL_SURFACE ( 'NONE', #5018, 10.00000000000000178 ) ;
#1533 = CARTESIAN_POINT ( 'NONE',  ( 2.740000000000000213, 0.5149999999999976819, 0.6774776749089244099 ) ) ;
#1534 = DIRECTION ( 'NONE',  ( 1.000000000000000000, -3.469446951953614189E-16, 0.000000000000000000 ) ) ;
#1535 = CARTESIAN_POINT ( 'NONE',  ( 0.5000000000000000000, 0.2499999999999982792, -1.911797424705720339 ) ) ;
#1536 = CARTESIAN_POINT ( 'NONE',  ( -45.00000000000002842, 15.00000000000000000, -44.99999999999998579 ) ) ;
#1537 = ORIENTED_EDGE ( 'NONE', *, *, #1872, .F. ) ;
#1538 = DIRECTION ( 'NONE',  ( -0.000000000000000000, -0.000000000000000000, 1.000000000000000000 ) ) ;
#1539 = LINE ( 'NONE', #1964, #2554 ) ;
#1540 = UNCERTAINTY_MEASURE_WITH_UNIT (LENGTH_MEASURE( 1.000000000000000082E-05 ), #2550, 'distance_accuracy_value', 'NONE');
#1541 = AXIS2_PLACEMENT_3D ( 'NONE', #2073, #2521, #5804 ) ;
#1542 = VECTOR ( 'NONE', #1642, 1000.000000000000000 ) ;
#1543 = ADVANCED_FACE ( 'NONE', ( #3929 ), #2565, .T. ) ;
#1544 = ORIENTED_EDGE ( 'NONE', *, *, #1174, .T. ) ;
#1545 = CIRCLE ( 'NONE', #4752, 12.00000000000000000 ) ;
#1546 = VECTOR ( 'NONE', #3946, 1000.000000000000114 ) ;
#1547 = DIRECTION ( 'NONE',  ( 3.469446951953614189E-16, 1.000000000000000000, 1.734723475976808327E-16 ) ) ;
#1548 = CARTESIAN_POINT ( 'NONE',  ( 55.00000000000000711, 0.000000000000000000, -7.000000000000000000 ) ) ;
#1549 = AXIS2_PLACEMENT_3D ( 'NONE', #1035, #2891, #4297 ) ;
#1550 = CIRCLE ( 'NONE', #5524, 4.999999999999990230 ) ;
#1551 = DIRECTION ( 'NONE',  ( 0.000000000000000000, 0.000000000000000000, -1.000000000000000000 ) ) ;
#1552 = ORIENTED_EDGE ( 'NONE', *, *, #4555, .T. ) ;
#1553 = ORIENTED_EDGE ( 'NONE', *, *, #528, .F. ) ;
#1554 = CIRCLE ( 'NONE', #16, 5.000000000000000000 ) ;
#1555 = DIRECTION ( 'NONE',  ( -3.469446951953614189E-16, -1.000000000000000000, -8.673617379884041635E-17 ) ) ;
#1556 = DIRECTION ( 'NONE',  ( 0.000000000000000000, 1.000000000000000000, 0.000000000000000000 ) ) ;
#1557 = ORIENTED_EDGE ( 'NONE', *, *, #1523, .F. ) ;
#1558 = AXIS2_PLACEMENT_3D ( 'NONE', #2443, #1528, #4423 ) ;
#1559 = CIRCLE ( 'NONE', #5347, 10.00000000000000178 ) ;
#1560 = DIRECTION ( 'NONE',  ( 2.312964634635742895E-17, 1.000000000000000000, -0.000000000000000000 ) ) ;
#1561 = CARTESIAN_POINT ( 'NONE',  ( 0.000000000000000000, 15.00000000000000000, 0.000000000000000000 ) ) ;
#1562 = DIRECTION ( 'NONE',  ( 0.000000000000000000, 0.000000000000000000, 1.000000000000000000 ) ) ;
#1563 = VERTEX_POINT ( 'NONE', #3901 ) ;
#1564 = VECTOR ( 'NONE', #532, 1000.000000000000000 ) ;
#1565 = CARTESIAN_POINT ( 'NONE',  ( 37.50000000000000711, 6.288372600415927295E-15, 75.00000000000000000 ) ) ;
#1566 = CIRCLE ( 'NONE', #597, 7.000000000000000000 ) ;
#1567 = DIRECTION ( 'NONE',  ( 1.000000000000000000, 0.000000000000000000, 0.000000000000000000 ) ) ;
#1568 = EDGE_CURVE ( 'NONE', #2772, #5459, #5846, .T. ) ;
#1569 = PLANE ( 'NONE',  #4280 ) ;
#1570 = DIRECTION ( 'NONE',  ( -1.000000000000000000, 0.000000000000000000, 0.000000000000000000 ) ) ;
#1571 = CIRCLE ( 'NONE', #3608, 1.934182851860892116 ) ;
#1572 = LINE ( 'NONE', #2940, #5440 ) ;
#1573 = EDGE_CURVE ( 'NONE', #939, #3970, #2780, .T. ) ;
#1575 =( GEOMETRIC_REPRESENTATION_CONTEXT ( 3 ) GLOBAL_UNCERTAINTY_ASSIGNED_CONTEXT ( ( #4283 ) ) GLOBAL_UNIT_ASSIGNED_CONTEXT ( ( #1212, #2577, #2121 ) ) REPRESENTATION_CONTEXT ( 'NONE', 'WORKASPACE' ) );
#1574 = DIRECTION ( 'NONE',  ( 1.000000000000000000, -4.770489558936219510E-17, 0.000000000000000000 ) ) ;
#1576 = VERTEX_POINT ( 'NONE', #4364 ) ;
#1577 = ORIENTED_EDGE ( 'NONE', *, *, #3496, .F. ) ;
#1578 = DIRECTION ( 'NONE',  ( 1.000000000000000000, 0.000000000000000000, 0.000000000000000000 ) ) ;
#1579 = AXIS2_PLACEMENT_3D ( 'NONE', #3650, #941, #5113 ) ;
#1580 = COLOUR_RGB ( '',0.8941176470588234615, 0.8941176470588234615, 0.8941176470588234615 ) ;
#1581 = ORIENTED_EDGE ( 'NONE', *, *, #3788, .T. ) ;
#1582 = SURFACE_SIDE_STYLE ('',( #3883 ) ) ;
#1583 = EDGE_CURVE ( 'NONE', #1856, #2744, #1202, .T. ) ;
#1584 = FACE_OUTER_BOUND ( 'NONE', #543, .T. ) ;
#1585 = VECTOR ( 'NONE', #129, 1000.000000000000000 ) ;
#1586 = AXIS2_PLACEMENT_3D ( 'NONE', #5548, #3300, #1896 ) ;
#1587 = DIRECTION ( 'NONE',  ( 0.000000000000000000, 0.000000000000000000, 1.000000000000000000 ) ) ;
#1588 = VERTEX_POINT ( 'NONE', #5784 ) ;
#1589 = ORIENTED_EDGE ( 'NONE', *, *, #5731, .T. ) ;
#1590 = CARTESIAN_POINT ( 'NONE',  ( -74.99999999999998579, -15.00000000000000000, 75.00000000000000000 ) ) ;
#1591 = CARTESIAN_POINT ( 'NONE',  ( 75.00000000000001421, -15.00000000000000355, -75.00000000000000000 ) ) ;
#1592 = ORIENTED_EDGE ( 'NONE', *, *, #3425, .T. ) ;
#1593 = CARTESIAN_POINT ( 'NONE',  ( 137.4999999999999716, 0.000000000000000000, -7.000000000000000000 ) ) ;
#1594 = CYLINDRICAL_SURFACE ( 'NONE', #4674, 5.499999999999991118 ) ;
#1595 = CARTESIAN_POINT ( 'NONE',  ( 7.345657149124338758, 1.312408941150044583, 0.000000000000000000 ) ) ;
#1596 = ORIENTED_EDGE ( 'NONE', *, *, #2092, .F. ) ;
#1597 = FACE_OUTER_BOUND ( 'NONE', #4974, .T. ) ;
#1598 = CARTESIAN_POINT ( 'NONE',  ( 162.5000000000000000, 15.00000000000000000, 75.00000000000001421 ) ) ;
#1599 = CARTESIAN_POINT ( 'NONE',  ( 3.700000000000000178, 0.000000000000000000, 0.000000000000000000 ) ) ;
#1600 = LINE ( 'NONE', #2905, #2927 ) ;
#1601 = DIRECTION ( 'NONE',  ( 1.000000000000000000, 0.000000000000000000, 0.000000000000000000 ) ) ;
#1602 = EDGE_LOOP ( 'NONE', ( #662, #1338, #4474, #4542, #4506 ) ) ;
#1603 = CYLINDRICAL_SURFACE ( 'NONE', #5433, 0.9999999999999991118 ) ;
#1604 = B_SPLINE_CURVE_WITH_KNOTS ( 'NONE', 3,
 ( #257, #2095, #1021, #2742 ),
 .UNSPECIFIED., .F., .F.,
 ( 4, 4 ),
 ( 0.004656695506220393486, 0.007337072593346777132 ),
 .UNSPECIFIED. ) ;
#1605 = FILL_AREA_STYLE ('',( #2060 ) ) ;
#1606 = LINE ( 'NONE', #5820, #5473 ) ;
#1607 = UNCERTAINTY_MEASURE_WITH_UNIT (LENGTH_MEASURE( 1.000000000000000082E-05 ), #5602, 'distance_accuracy_value', 'NONE');
#1608 = PRODUCT_DEFINITION_CONTEXT ( 'detailed design', #790, 'design' ) ;
#1609 = ORIENTED_EDGE ( 'NONE', *, *, #4675, .T. ) ;
#1610 = EDGE_CURVE ( 'NONE', #3914, #3739, #4338, .T. ) ;
#1611 = AXIS2_PLACEMENT_3D ( 'NONE', #74, #3401, #2430 ) ;
#1612 = EDGE_CURVE ( 'NONE', #5526, #1289, #5877, .T. ) ;
#1613 = AXIS2_PLACEMENT_3D ( 'NONE', #2411, #1020, #5661 ) ;
#1614 = LINE ( 'NONE', #3974, #2317 ) ;
#1615 = EDGE_CURVE ( 'NONE', #4278, #5342, #644, .T. ) ;
#1616 = DIRECTION ( 'NONE',  ( 1.000000000000000000, 0.000000000000000000, 0.000000000000000000 ) ) ;
#1617 = EDGE_CURVE ( 'NONE', #805, #171, #1517, .T. ) ;
#1618 = ORIENTED_EDGE ( 'NONE', *, *, #694, .T. ) ;
#1619 = ORIENTED_EDGE ( 'NONE', *, *, #491, .F. ) ;
#1620 = CYLINDRICAL_SURFACE ( 'NONE', #5826, 5.000000000000004441 ) ;
#1621 = DIRECTION ( 'NONE',  ( 1.000000000000000000, 0.000000000000000000, 0.000000000000000000 ) ) ;
#1622 = ORIENTED_EDGE ( 'NONE', *, *, #2648, .F. ) ;
#1623 = CARTESIAN_POINT ( 'NONE',  ( 62.50000000000001421, -1.951563910473909559E-15, 55.00000000000000000 ) ) ;
#1624 = ADVANCED_FACE ( 'NONE', ( #5305 ), #2592, .F. ) ;
#1625 = CARTESIAN_POINT ( 'NONE',  ( 67.00000000000001421, 0.000000000000000000, -5.000000000000000000 ) ) ;
#1626 = CARTESIAN_POINT ( 'NONE',  ( 66.39913938277356920, 0.000000000000000000, -9.500000000000000000 ) ) ;
#1627 = EDGE_LOOP ( 'NONE', ( #3281, #4685, #731, #4014 ) ) ;
#1628 = APPLICATION_PROTOCOL_DEFINITION ( 'draft international standard', 'automotive_design', 1998, #3887 ) ;
#1629 = DIRECTION ( 'NONE',  ( -0.8949343913984706411, 0.4461977533473793223, 0.000000000000000000 ) ) ;
#1630 = LINE ( 'NONE', #5367, #1458 ) ;
#1631 = CARTESIAN_POINT ( 'NONE',  ( 0.5477065543514070267, 2.408992218395923449E-16, 1.934182851860892116 ) ) ;
#1632 = DIRECTION ( 'NONE',  ( 0.000000000000000000, 0.000000000000000000, -1.000000000000000000 ) ) ;
#1633 = DIRECTION ( 'NONE',  ( 0.000000000000000000, 0.000000000000000000, 1.000000000000000000 ) ) ;
#1634 = ORIENTED_EDGE ( 'NONE', *, *, #2645, .T. ) ;
#1635 = PRODUCT ( 'slotted pan head screw_iso_ISO 1580 - M2 x 8 - 8N', 'slotted pan head screw_iso_ISO 1580 - M2 x 8 - 8N', '', ( #515 ) ) ;
#1636 = ORIENTED_EDGE ( 'NONE', *, *, #491, .T. ) ;
#1637 = SURFACE_STYLE_USAGE ( .BOTH. , #5312 ) ;
#1638 = DIRECTION ( 'NONE',  ( 0.000000000000000000, 0.000000000000000000, 1.000000000000000000 ) ) ;
#1639 = ORIENTED_EDGE ( 'NONE', *, *, #2435, .T. ) ;
#1640 = AXIS2_PLACEMENT_3D ( 'NONE', #1230, #1744, #3085 ) ;
#1641 = EDGE_CURVE ( 'NONE', #553, #3979, #1416, .T. ) ;
#1642 = DIRECTION ( 'NONE',  ( 1.000000000000000000, -0.000000000000000000, -0.000000000000000000 ) ) ;
#1643 = EDGE_CURVE ( 'NONE', #1327, #4518, #3174, .T. ) ;
#1644 = CARTESIAN_POINT ( 'NONE',  ( 37.50000000000000711, 6.288372600415927295E-15, 71.29999999999999716 ) ) ;
#1645 =( GEOMETRIC_REPRESENTATION_CONTEXT ( 3 ) GLOBAL_UNCERTAINTY_ASSIGNED_CONTEXT ( ( #1116 ) ) GLOBAL_UNIT_ASSIGNED_CONTEXT ( ( #1219, #1735, #1190 ) ) REPRESENTATION_CONTEXT ( 'NONE', 'WORKASPACE' ) );
#1647 = ORIENTED_EDGE ( 'NONE', *, *, #642, .F. ) ;
#1646 = EDGE_CURVE ( 'NONE', #2345, #1926, #4025, .T. ) ;
#1648 = ORIENTED_EDGE ( 'NONE', *, *, #1008, .F. ) ;
#1649 = FACE_OUTER_BOUND ( 'NONE', #3772, .T. ) ;
#1650 = AXIS2_PLACEMENT_3D ( 'NONE', #5756, #3905, #748 ) ;
#1651 = DIRECTION ( 'NONE',  ( 0.000000000000000000, -3.612465276695121047E-15, 1.000000000000000000 ) ) ;
#1652 = EDGE_LOOP ( 'NONE', ( #3751, #3779 ) ) ;
#1653 = DIRECTION ( 'NONE',  ( 0.000000000000000000, -0.000000000000000000, 1.000000000000000000 ) ) ;
#1654 = CARTESIAN_POINT ( 'NONE',  ( 162.5000000000000000, 15.00000000000000000, 75.00000000000001421 ) ) ;
#1655 = PRESENTATION_LAYER_ASSIGNMENT (  '', '', ( #5611 ) ) ;
#1656 = CARTESIAN_POINT ( 'NONE',  ( 0.3226060873438262311, -0.5149999999999915756, -2.189154565102686245 ) ) ;
#1657 = AXIS2_PLACEMENT_3D ( 'NONE', #3859, #1193, #2931 ) ;
#1658 = EDGE_LOOP ( 'NONE', ( #1048, #3597, #2673, #5918 ) ) ;
#1659 = EDGE_CURVE ( 'NONE', #111, #377, #88, .T. ) ;
#1660 = DIRECTION ( 'NONE',  ( 0.000000000000000000, 0.000000000000000000, -1.000000000000000000 ) ) ;
#1661 = AXIS2_PLACEMENT_3D ( 'NONE', #2869, #1017, #1352 ) ;
#1662 = AXIS2_PLACEMENT_3D ( 'NONE', #2567, #2473, #179 ) ;
#1663 = DIRECTION ( 'NONE',  ( 0.000000000000000000, 0.000000000000000000, 1.000000000000000000 ) ) ;
#1664 = DIRECTION ( 'NONE',  ( 1.000000000000000000, 0.000000000000000000, 0.000000000000000000 ) ) ;
#1665 = CARTESIAN_POINT ( 'NONE',  ( 3.700000000000000178, 2.500000000000000000, 0.000000000000000000 ) ) ;
#1666 = DIRECTION ( 'NONE',  ( 0.000000000000000000, -1.000000000000000000, 0.000000000000000000 ) ) ;
#1667 = ORIENTED_EDGE ( 'NONE', *, *, #761, .T. ) ;
#1668 = AXIS2_PLACEMENT_3D ( 'NONE', #2053, #152, #1632 ) ;
#1669 = CIRCLE ( 'NONE', #5920, 2.649999999999999467 ) ;
#1670 = FACE_OUTER_BOUND ( 'NONE', #1860, .T. ) ;
#1671 = AXIS2_PLACEMENT_3D ( 'NONE', #160, #4228, #5194 ) ;
#1672 = VECTOR ( 'NONE', #1137, 1000.000000000000000 ) ;
#1673 = ORIENTED_EDGE ( 'NONE', *, *, #5391, .T. ) ;
#1674 = B_SPLINE_CURVE_WITH_KNOTS ( 'NONE', 3,
 ( #143, #5178, #5541, #4268 ),
 .UNSPECIFIED., .F., .F.,
 ( 4, 4 ),
 ( 0.001586480565025038831, 0.004268227387428736967 ),
 .UNSPECIFIED. ) ;
#1675 =( NAMED_UNIT ( * ) PLANE_ANGLE_UNIT ( ) SI_UNIT ( $, .RADIAN. ) );
#1676 = LINE ( 'NONE', #2512, #2220 ) ;
#1677 = CARTESIAN_POINT ( 'NONE',  ( -49.33012701892221230, 45.00000000000000000, 37.50000000000000000 ) ) ;
#1678 = COLOUR_RGB ( '',1.000000000000000000, 0.9490196078431372140, 0.9098039215686274384 ) ;
#1679 = VERTEX_POINT ( 'NONE', #4000 ) ;
#1680 = VERTEX_POINT ( 'NONE', #424 ) ;
#1681 = SURFACE_STYLE_FILL_AREA ( #737 ) ;
#1682 = AXIS2_PLACEMENT_3D ( 'NONE', #2047, #4335, #2012 ) ;
#1683 = ORIENTED_EDGE ( 'NONE', *, *, #3427, .T. ) ;
#1684 = DIRECTION ( 'NONE',  ( 0.000000000000000000, 1.000000000000000000, 0.000000000000000000 ) ) ;
#1685 = LINE ( 'NONE', #804, #3310 ) ;
#1686 = VERTEX_POINT ( 'NONE', #3155 ) ;
#1687 = FACE_OUTER_BOUND ( 'NONE', #5817, .T. ) ;
#1688 = EDGE_CURVE ( 'NONE', #5283, #3078, #1336, .T. ) ;
#1689 = ORIENTED_EDGE ( 'NONE', *, *, #3248, .F. ) ;
#1690 = DIRECTION ( 'NONE',  ( -0.4999999999999993339, 0.000000000000000000, 0.8660254037844389297 ) ) ;
#1691 = CARTESIAN_POINT ( 'NONE',  ( -35.00000000000000711, 40.00000000000000000, -45.00000000000000000 ) ) ;
#1692 = DIRECTION ( 'NONE',  ( 1.000000000000000000, -0.000000000000000000, 0.000000000000000000 ) ) ;
#1693 = PRODUCT_DEFINITION_CONTEXT ( 'detailed design', #2734, 'design' ) ;
#1694 = DIRECTION ( 'NONE',  ( -0.000000000000000000, -1.000000000000000000, -0.000000000000000000 ) ) ;
#1695 = FACE_BOUND ( 'NONE', #1062, .T. ) ;
#1696 = EDGE_CURVE ( 'NONE', #1436, #764, #5512, .T. ) ;
#1697 = EDGE_LOOP ( 'NONE', ( #2070, #4371, #5360, #922 ) ) ;
#1698 = DIRECTION ( 'NONE',  ( 0.000000000000000000, 1.224646799147353207E-16, -1.000000000000000000 ) ) ;
#1699 = VERTEX_POINT ( 'NONE', #5897 ) ;
#1700 = CARTESIAN_POINT ( 'NONE',  ( 75.00000000000001421, 0.000000000000000000, 0.000000000000000000 ) ) ;
#1701 = PRODUCT_DEFINITION_SHAPE ( 'NONE', 'NONE',  #2570 ) ;
#1702 = CARTESIAN_POINT ( 'NONE',  ( 75.00000000000001421, -7.000000000000007105, 75.00000000000000000 ) ) ;
#1703 = DIRECTION ( 'NONE',  ( 0.000000000000000000, -1.000000000000000000, 0.000000000000000000 ) ) ;
#1704 = EDGE_LOOP ( 'NONE', ( #948, #3524, #962, #5311 ) ) ;
#1705 = VERTEX_POINT ( 'NONE', #5935 ) ;
#1706 = CYLINDRICAL_SURFACE ( 'NONE', #5712, 5.000000000000004441 ) ;
#1707 = CARTESIAN_POINT ( 'NONE',  ( 35.00000000000000000, 6.594534300202765954E-15, 55.00000000000000000 ) ) ;
#1708 = VERTEX_POINT ( 'NONE', #5394 ) ;
#1709 = CARTESIAN_POINT ( 'NONE',  ( 224.9999999999999716, 6.999999999999985789, 75.00000000000000000 ) ) ;
#1710 = DIRECTION ( 'NONE',  ( 0.000000000000000000, 0.000000000000000000, 1.000000000000000000 ) ) ;
#1711 = EDGE_LOOP ( 'NONE', ( #2373, #5638, #896, #4217 ) ) ;
#1712 = CARTESIAN_POINT ( 'NONE',  ( 0.04978537780227577231, -0.2499999999999997224, -1.594765474869573874 ) ) ;
#1713 = ORIENTED_EDGE ( 'NONE', *, *, #4593, .F. ) ;
#1714 = EDGE_CURVE ( 'NONE', #3630, #1472, #606, .T. ) ;
#1715 = EDGE_CURVE ( 'NONE', #2159, #5534, #4295, .T. ) ;
#1716 = CARTESIAN_POINT ( 'NONE',  ( 1.794155980045911036, 0.000000000000000000, 0.000000000000000000 ) ) ;
#1717 = EDGE_CURVE ( 'NONE', #2658, #5946, #2347, .T. ) ;
#1718 =( REPRESENTATION_RELATIONSHIP ('NONE','NONE', #5609, #951 ) REPRESENTATION_RELATIONSHIP_WITH_TRANSFORMATION ( #4259 )SHAPE_REPRESENTATION_RELATIONSHIP( ) );
#1719 = CARTESIAN_POINT ( 'NONE',  ( 25.00000000000000711, 7.000000000000011546, 65.00000000000000000 ) ) ;
#1720 = CARTESIAN_POINT ( 'NONE',  ( 62.50000000000001421, -1.951563910473909559E-15, 65.00000000000000000 ) ) ;
#1721 = DIRECTION ( 'NONE',  ( 0.000000000000000000, 1.000000000000000000, -0.000000000000000000 ) ) ;
#1722 = EDGE_LOOP ( 'NONE', ( #4931, #1841, #3678, #5341 ) ) ;
#1723 = EDGE_CURVE ( 'NONE', #3307, #3568, #2735, .T. ) ;
#1724 = DIRECTION ( 'NONE',  ( -0.000000000000000000, -0.000000000000000000, 1.000000000000000000 ) ) ;
#1725 = VERTEX_POINT ( 'NONE', #4049 ) ;
#1726 = DIRECTION ( 'NONE',  ( 1.000000000000000000, 0.000000000000000000, 0.000000000000000000 ) ) ;
#1727 = SURFACE_STYLE_FILL_AREA ( #373 ) ;
#1728 = DIRECTION ( 'NONE',  ( 0.000000000000000000, 0.000000000000000000, -1.000000000000000000 ) ) ;
#1729 = EDGE_CURVE ( 'NONE', #1825, #1750, #2196, .T. ) ;
#1730 = LINE ( 'NONE', #5352, #5232 ) ;
#1731 = ORIENTED_EDGE ( 'NONE', *, *, #2906, .T. ) ;
#1732 = AXIS2_PLACEMENT_3D ( 'NONE', #2985, #4838, #678 ) ;
#1733 = ORIENTED_EDGE ( 'NONE', *, *, #1895, .F. ) ;
#1734 = AXIS2_PLACEMENT_3D ( 'NONE', #1145, #1094, #2515 ) ;
#1735 =( NAMED_UNIT ( * ) PLANE_ANGLE_UNIT ( ) SI_UNIT ( $, .RADIAN. ) );
#1736 = ORIENTED_EDGE ( 'NONE', *, *, #2058, .F. ) ;
#1737 = DIRECTION ( 'NONE',  ( 0.000000000000000000, 0.000000000000000000, -1.000000000000000000 ) ) ;
#1738 = LINE ( 'NONE', #2102, #4679 ) ;
#1739 = ORIENTED_EDGE ( 'NONE', *, *, #1097, .T. ) ;
#1740 = DIRECTION ( 'NONE',  ( 1.007709689656716938E-16, 1.153406566473941260E-16, -1.000000000000000000 ) ) ;
#1741 = VERTEX_POINT ( 'NONE', #337 ) ;
#1742 = VECTOR ( 'NONE', #822, 1000.000000000000000 ) ;
#1743 = CARTESIAN_POINT ( 'NONE',  ( 75.00000000000001421, 0.000000000000000000, 9.500000000000000000 ) ) ;
#1744 = DIRECTION ( 'NONE',  ( 0.000000000000000000, 1.000000000000000000, 0.000000000000000000 ) ) ;
#1745 = AXIS2_PLACEMENT_3D ( 'NONE', #530, #82, #5327 ) ;
#1746 = CARTESIAN_POINT ( 'NONE',  ( 137.4999999999999716, -15.00000000000000000, 75.00000000000001421 ) ) ;
#1747 = UNCERTAINTY_MEASURE_WITH_UNIT (LENGTH_MEASURE( 1.000000000000000082E-05 ), #5783, 'distance_accuracy_value', 'NONE');
#1748 = CYLINDRICAL_SURFACE ( 'NONE', #3511, 10.00000000000000178 ) ;
#1749 = CYLINDRICAL_SURFACE ( 'NONE', #3981, 2.500000000000002220 ) ;
#1750 = VERTEX_POINT ( 'NONE', #3569 ) ;
#1751 = EDGE_CURVE ( 'NONE', #3368, #605, #4825, .T. ) ;
#1752 = CIRCLE ( 'NONE', #3881, 5.000000000000004441 ) ;
#1753 =( LENGTH_UNIT ( ) NAMED_UNIT ( * ) SI_UNIT ( .MILLI., .METRE. ) );
#1754 = VECTOR ( 'NONE', #115, 1000.000000000000000 ) ;
#1755 = CARTESIAN_POINT ( 'NONE',  ( -25.39999999999996305, 5.817072295949926440E-16, -4.749999999999999112 ) ) ;
#1756 = EDGE_CURVE ( 'NONE', #5556, #4755, #1418, .T. ) ;
#1757 = VERTEX_POINT ( 'NONE', #3120 ) ;
#1758 = AXIS2_PLACEMENT_3D ( 'NONE', #683, #5330, #2044 ) ;
#1760 = AXIS2_PLACEMENT_3D ( 'NONE', #5478, #4690, #523 ) ;
#1759 = FACE_OUTER_BOUND ( 'NONE', #3035, .T. ) ;
#1761 =( LENGTH_UNIT ( ) NAMED_UNIT ( * ) SI_UNIT ( .MILLI., .METRE. ) );
#1762 = CARTESIAN_POINT ( 'NONE',  ( 65.00000000000001421, -1.951563910473909559E-15, 55.00000000000000000 ) ) ;
#1763 = VECTOR ( 'NONE', #3641, 1000.000000000000000 ) ;
#1764 = DIRECTION ( 'NONE',  ( 1.000000000000000000, -0.000000000000000000, 0.000000000000000000 ) ) ;
#1765 = EDGE_CURVE ( 'NONE', #2341, #1155, #3185, .T. ) ;
#1766 = CIRCLE ( 'NONE', #4590, 8.000000000000000000 ) ;
#1767 = AXIS2_PLACEMENT_3D ( 'NONE', #3848, #3734, #2368 ) ;
#1768 = ORIENTED_EDGE ( 'NONE', *, *, #1729, .F. ) ;
#1769 = ADVANCED_FACE ( 'NONE', ( #4980 ), #4547, .F. ) ;
#1770 = VERTEX_POINT ( 'NONE', #5871 ) ;
#1771 = DIRECTION ( 'NONE',  ( 0.000000000000000000, 0.000000000000000000, -1.000000000000000000 ) ) ;
#1772 =( NAMED_UNIT ( * ) PLANE_ANGLE_UNIT ( ) SI_UNIT ( $, .RADIAN. ) );
#1773 = VERTEX_POINT ( 'NONE', #1691 ) ;
#1774 = CARTESIAN_POINT ( 'NONE',  ( 0.000000000000000000, 0.000000000000000000, -1.886264737416298409 ) ) ;
#1775 = DIRECTION ( 'NONE',  ( -0.000000000000000000, -0.000000000000000000, -1.000000000000000000 ) ) ;
#1776 = ORIENTED_EDGE ( 'NONE', *, *, #611, .T. ) ;
#1777 = CARTESIAN_POINT ( 'NONE',  ( 137.4999999999999716, 15.00000000000000000, 75.00000000000001421 ) ) ;
#1778 = ORIENTED_EDGE ( 'NONE', *, *, #5908, .F. ) ;
#1779 =( GEOMETRIC_REPRESENTATION_CONTEXT ( 3 ) GLOBAL_UNCERTAINTY_ASSIGNED_CONTEXT ( ( #2595 ) ) GLOBAL_UNIT_ASSIGNED_CONTEXT ( ( #3361, #86, #3696 ) ) REPRESENTATION_CONTEXT ( 'NONE', 'WORKASPACE' ) );
#1780 = DIRECTION ( 'NONE',  ( 0.000000000000000000, 1.000000000000000000, -0.000000000000000000 ) ) ;
#1781 = DIRECTION ( 'NONE',  ( 1.000000000000000000, 0.000000000000000000, -0.000000000000000000 ) ) ;
#1782 = DIRECTION ( 'NONE',  ( -0.000000000000000000, 0.000000000000000000, 1.000000000000000000 ) ) ;
#1783 = CARTESIAN_POINT ( 'NONE',  ( -49.33012701892221230, 40.00000000000000000, 52.49999999999999289 ) ) ;
#1784 = ORIENTED_EDGE ( 'NONE', *, *, #5319, .F. ) ;
#1785 = CARTESIAN_POINT ( 'NONE',  ( -74.99999999999998579, 15.00000000000000000, 75.00000000000000000 ) ) ;
#1786 = ORIENTED_EDGE ( 'NONE', *, *, #203, .F. ) ;
#1787 = DIRECTION ( 'NONE',  ( 0.000000000000000000, 0.000000000000000000, 1.000000000000000000 ) ) ;
#1788 = PRODUCT_RELATED_PRODUCT_CATEGORY ( 'part', '', ( #58 ) ) ;
#1789 = DIRECTION ( 'NONE',  ( 0.000000000000000000, -1.734723475976808080E-16, -1.000000000000000000 ) ) ;
#1790 = EDGE_CURVE ( 'NONE', #3934, #1757, #2416, .T. ) ;
#1791 = EDGE_CURVE ( 'NONE', #3262, #2126, #4120, .T. ) ;
#1792 = LINE ( 'NONE', #1506, #2327 ) ;
#1793 = ORIENTED_EDGE ( 'NONE', *, *, #3169, .F. ) ;
#1794 = VERTEX_POINT ( 'NONE', #389 ) ;
#1795 = ADVANCED_FACE ( 'NONE', ( #3601 ), #4578, .T. ) ;
#1796 = DIRECTION ( 'NONE',  ( 0.000000000000000000, 0.000000000000000000, -1.000000000000000000 ) ) ;
#1797 = APPLICATION_CONTEXT ( 'automotive_design' ) ;
#1798 = ORIENTED_EDGE ( 'NONE', *, *, #3461, .T. ) ;
#1799 = PLANE ( 'NONE',  #4574 ) ;
#1800 = DIRECTION ( 'NONE',  ( 0.000000000000000000, 0.000000000000000000, 1.000000000000000000 ) ) ;
#1801 = ORIENTED_EDGE ( 'NONE', *, *, #5050, .T. ) ;
#1802 = CARTESIAN_POINT ( 'NONE',  ( 68.00000000000000000, -1.951563910473909559E-15, 71.29999999999999716 ) ) ;
#1803 = ORIENTED_EDGE ( 'NONE', *, *, #2289, .T. ) ;
#1804 = CARTESIAN_POINT ( 'NONE',  ( 75.00000000000001421, 0.000000000000000000, 0.000000000000000000 ) ) ;
#1805 = EDGE_CURVE ( 'NONE', #3531, #5881, #2606, .T. ) ;
#1806 = CARTESIAN_POINT ( 'NONE',  ( 3.900000000000000799, 0.000000000000000000, 0.000000000000000000 ) ) ;
#1807 = DIRECTION ( 'NONE',  ( -0.000000000000000000, -0.000000000000000000, 1.000000000000000000 ) ) ;
#1808 = VECTOR ( 'NONE', #1133, 1000.000000000000000 ) ;
#1809 = FACE_OUTER_BOUND ( 'NONE', #395, .T. ) ;
#1810 = CARTESIAN_POINT ( 'NONE',  ( 75.00000000000001421, 1.469576158976823947E-15, -12.00000000000000000 ) ) ;
#1811 = EDGE_LOOP ( 'NONE', ( #569, #4895 ) ) ;
#1812 = DIRECTION ( 'NONE',  ( -0.000000000000000000, 0.000000000000000000, 1.000000000000000000 ) ) ;
#1813 = VERTEX_POINT ( 'NONE', #1496 ) ;
#1814 = CARTESIAN_POINT ( 'NONE',  ( 75.00000000000001421, -7.000000000000007105, -75.00000000000000000 ) ) ;
#1815 = VECTOR ( 'NONE', #2977, 1000.000000000000000 ) ;
#1816 = FACE_OUTER_BOUND ( 'NONE', #2349, .T. ) ;
#1817 = DIRECTION ( 'NONE',  ( -0.000000000000000000, -0.000000000000000000, 1.000000000000000000 ) ) ;
#1818 = EDGE_LOOP ( 'NONE', ( #1199, #4772, #2611, #1887 ) ) ;
#1819 = EDGE_CURVE ( 'NONE', #467, #3160, #3328, .T. ) ;
#1820 = VERTEX_POINT ( 'NONE', #2294 ) ;
#1821 = DIRECTION ( 'NONE',  ( -0.000000000000000000, 0.000000000000000000, 1.000000000000000000 ) ) ;
#1822 = ITEM_DEFINED_TRANSFORMATION ( 'NONE', 'NONE', #2265,  #5080 ) ;
#1823 = EDGE_CURVE ( 'NONE', #2749, #2650, #2502, .T. ) ;
#1824 = CARTESIAN_POINT ( 'NONE',  ( 37.50000000000000711, 6.288372600415927295E-15, 55.00000000000000000 ) ) ;
#1825 = VERTEX_POINT ( 'NONE', #2318 ) ;
#1826 = B_SPLINE_CURVE_WITH_KNOTS ( 'NONE', 3,
 ( #4276, #2363, #1442, #3304, #997, #1901 ),
 .UNSPECIFIED., .F., .F.,
 ( 4, 2, 4 ),
 ( 0.002363858439908544419, 0.002786031303543298580, 0.003208204167178053175 ),
 .UNSPECIFIED. ) ;
#1827 = EDGE_CURVE ( 'NONE', #2491, #3503, #4742, .T. ) ;
#1828 = CARTESIAN_POINT ( 'NONE',  ( 0.000000000000000000, 2.350000000000000089, 0.5149999999999996803 ) ) ;
#1829 = CARTESIAN_POINT ( 'NONE',  ( -49.33012701892221230, 40.00000000000000000, 52.49999999999999289 ) ) ;
#1830 = VERTEX_POINT ( 'NONE', #950 ) ;
#1831 = ORIENTED_EDGE ( 'NONE', *, *, #1306, .T. ) ;
#1832 = FACE_OUTER_BOUND ( 'NONE', #292, .T. ) ;
#1833 = AXIS2_PLACEMENT_3D ( 'NONE', #3894, #1621, #3443 ) ;
#1834 = CARTESIAN_POINT ( 'NONE',  ( 25.00000000000000711, -6.999999999999988454, 65.00000000000000000 ) ) ;
#1835 = DIRECTION ( 'NONE',  ( 1.000000000000000000, 0.000000000000000000, 0.000000000000000000 ) ) ;
#1836 = DIRECTION ( 'NONE',  ( 0.000000000000000000, 0.000000000000000000, -1.000000000000000000 ) ) ;
#1837 = CIRCLE ( 'NONE', #874, 0.9999999999999991118 ) ;
#1838 = PRODUCT_DEFINITION_SHAPE ( 'NONE', 'NONE',  #5981 ) ;
#1839 = DIRECTION ( 'NONE',  ( 1.000000000000000000, -0.000000000000000000, -0.000000000000000000 ) ) ;
#1840 =( GEOMETRIC_REPRESENTATION_CONTEXT ( 3 ) GLOBAL_UNCERTAINTY_ASSIGNED_CONTEXT ( ( #3846 ) ) GLOBAL_UNIT_ASSIGNED_CONTEXT ( ( #3319, #2371, #1883 ) ) REPRESENTATION_CONTEXT ( 'NONE', 'WORKASPACE' ) );
#1841 = ORIENTED_EDGE ( 'NONE', *, *, #4349, .T. ) ;
#1842 = EDGE_CURVE ( 'NONE', #553, #1750, #4665, .T. ) ;
#1843 = DIRECTION ( 'NONE',  ( 1.000000000000000000, 0.000000000000000000, 0.000000000000000000 ) ) ;
#1844 = FACE_OUTER_BOUND ( 'NONE', #4281, .T. ) ;
#1845 = VECTOR ( 'NONE', #566, 1000.000000000000000 ) ;
#1846 = CARTESIAN_POINT ( 'NONE',  ( 75.00000000000001421, -7.000000000000006217, 65.00000000000000000 ) ) ;
#1847 = CIRCLE ( 'NONE', #1063, 5.499999999999991118 ) ;
#1848 = CARTESIAN_POINT ( 'NONE',  ( 75.00000000000001421, 0.000000000000000000, 8.500000000000000000 ) ) ;
#1849 = AXIS2_PLACEMENT_3D ( 'NONE', #5851, #1721, #3744 ) ;
#1850 = CIRCLE ( 'NONE', #4965, 0.9999999999999991118 ) ;
#1851 = ORIENTED_EDGE ( 'NONE', *, *, #2278, .F. ) ;
#1852 = AXIS2_PLACEMENT_3D ( 'NONE', #381, #1288, #4910 ) ;
#1853 = DIRECTION ( 'NONE',  ( 0.000000000000000000, 0.000000000000000000, 1.000000000000000000 ) ) ;
#1854 = CONTEXT_DEPENDENT_SHAPE_REPRESENTATION ( #867, #533 ) ;
#1855 = DIRECTION ( 'NONE',  ( -0.000000000000000000, -1.000000000000000000, -0.000000000000000000 ) ) ;
#1856 = VERTEX_POINT ( 'NONE', #5565 ) ;
#1857 = AXIS2_PLACEMENT_3D ( 'NONE', #953, #2320, #2380 ) ;
#1858 = AXIS2_PLACEMENT_3D ( 'NONE', #2816, #541, #933 ) ;
#1859 = CARTESIAN_POINT ( 'NONE',  ( 65.00000000000001421, -1.951563910473909559E-15, 65.00000000000000000 ) ) ;
#1860 = EDGE_LOOP ( 'NONE', ( #2516, #2216, #3733, #370 ) ) ;
#1861 = VERTEX_POINT ( 'NONE', #3292 ) ;
#1862 = VECTOR ( 'NONE', #1335, 1000.000000000000000 ) ;
#1863 = STYLED_ITEM ( 'NONE', ( #310 ), #5722 ) ;
#1864 = FACE_BOUND ( 'NONE', #4858, .T. ) ;
#1865 = DIRECTION ( 'NONE',  ( -0.000000000000000000, -1.000000000000000000, -0.000000000000000000 ) ) ;
#1866 = EDGE_CURVE ( 'NONE', #2395, #4390, #1382, .T. ) ;
#1867 = DIRECTION ( 'NONE',  ( 0.000000000000000000, 0.000000000000000000, 1.000000000000000000 ) ) ;
#1868 = CARTESIAN_POINT ( 'NONE',  ( 75.00000000000001421, -7.000000000000006217, -65.00000000000000000 ) ) ;
#1869 = ORIENTED_EDGE ( 'NONE', *, *, #3434, .F. ) ;
#1870 = LINE ( 'NONE', #1415, #1993 ) ;
#1871 = AXIS2_PLACEMENT_3D ( 'NONE', #3900, #1073, #627 ) ;
#1872 = EDGE_CURVE ( 'NONE', #2273, #695, #2807, .T. ) ;
#1873 = FACE_OUTER_BOUND ( 'NONE', #4, .T. ) ;
#1874 = AXIS2_PLACEMENT_3D ( 'NONE', #3127, #1812, #4155 ) ;
#1875 = VERTEX_POINT ( 'NONE', #4149 ) ;
#1876 = CARTESIAN_POINT ( 'NONE',  ( 150.0000000000000284, 15.00000000000000000, -45.00000000000000000 ) ) ;
#1877 = EDGE_CURVE ( 'NONE', #5450, #4416, #4698, .T. ) ;
#1878 = CLOSED_SHELL ( 'NONE', ( #3533, #1624, #3092, #1531, #3612, #3644, #540, #2608, #643, #4242 ) ) ;
#1879 = ORIENTED_EDGE ( 'NONE', *, *, #5132, .T. ) ;
#1880 = CARTESIAN_POINT ( 'NONE',  ( -45.00000000000001421, 30.00000000000000355, 45.00000000000000000 ) ) ;
#1881 = FACE_OUTER_BOUND ( 'NONE', #5376, .T. ) ;
#1882 = ADVANCED_BREP_SHAPE_REPRESENTATION ( '', ( #272, #5080 ), #5457 ) ;
#1883 =( NAMED_UNIT ( * ) SI_UNIT ( $, .STERADIAN. ) SOLID_ANGLE_UNIT ( ) );
#1884 = ORIENTED_EDGE ( 'NONE', *, *, #3687, .F. ) ;
#1885 = CARTESIAN_POINT ( 'NONE',  ( 172.5000000000000284, 0.000000000000000000, 0.000000000000000000 ) ) ;
#1886 = ORIENTED_EDGE ( 'NONE', *, *, #4664, .F. ) ;
#1887 = ORIENTED_EDGE ( 'NONE', *, *, #3941, .T. ) ;
#1888 = CARTESIAN_POINT ( 'NONE',  ( 0.000000000000000000, -0.2499999999999997780, -2.000000000000000000 ) ) ;
#1889 = LINE ( 'NONE', #3356, #3200 ) ;
#1890 = FACE_OUTER_BOUND ( 'NONE', #1697, .T. ) ;
#1891 = AXIS2_PLACEMENT_3D ( 'NONE', #2885, #4258, #5610 ) ;
#1892 = DIRECTION ( 'NONE',  ( -0.000000000000000000, 0.000000000000000000, -1.000000000000000000 ) ) ;
#1893 = DIRECTION ( 'NONE',  ( -0.000000000000000000, -1.000000000000000000, -0.000000000000000000 ) ) ;
#1894 = ORIENTED_EDGE ( 'NONE', *, *, #2488, .F. ) ;
#1895 = EDGE_CURVE ( 'NONE', #3756, #3278, #1432, .T. ) ;
#1896 = DIRECTION ( 'NONE',  ( 1.000000000000000000, 0.000000000000000000, 0.000000000000000000 ) ) ;
#1897 = EDGE_CURVE ( 'NONE', #500, #1083, #1889, .T. ) ;
#1898 = PLANE ( 'NONE',  #5578 ) ;
#1899 = EDGE_CURVE ( 'NONE', #736, #1175, #476, .T. ) ;
#1900 = EDGE_CURVE ( 'NONE', #1962, #708, #668, .T. ) ;
#1901 = CARTESIAN_POINT ( 'NONE',  ( 0.000000000000000000, 0.2499999999999982792, 1.312875263449799323 ) ) ;
#1902 = EDGE_LOOP ( 'NONE', ( #1886, #5125, #1486, #4835 ) ) ;
#1903 = FILL_AREA_STYLE ('',( #5191 ) ) ;
#1904 = CARTESIAN_POINT ( 'NONE',  ( 67.00000000000001421, 0.000000000000000000, 0.000000000000000000 ) ) ;
#1905 = VECTOR ( 'NONE', #4504, 1000.000000000000000 ) ;
#1906 = ORIENTED_EDGE ( 'NONE', *, *, #4132, .F. ) ;
#1907 = ADVANCED_FACE ( 'NONE', ( #4723 ), #1407, .F. ) ;
#1908 = CARTESIAN_POINT ( 'NONE',  ( -45.00000000000001421, 0.000000000000000000, 45.00000000000000000 ) ) ;
#1909 = CONTEXT_DEPENDENT_SHAPE_REPRESENTATION ( #4211, #4168 ) ;
#1910 = DIRECTION ( 'NONE',  ( 0.000000000000000000, 0.000000000000000000, 1.000000000000000000 ) ) ;
#1911 = ORIENTED_EDGE ( 'NONE', *, *, #3225, .T. ) ;
#1912 = ORIENTED_EDGE ( 'NONE', *, *, #5501, .T. ) ;
#1913 =( NAMED_UNIT ( * ) SI_UNIT ( $, .STERADIAN. ) SOLID_ANGLE_UNIT ( ) );
#1914 = CARTESIAN_POINT ( 'NONE',  ( 137.4999999999999716, 15.00000000000000000, 75.00000000000001421 ) ) ;
#1915 = CARTESIAN_POINT ( 'NONE',  ( -55.00000000000001421, 40.00000000000000000, 45.00000000000000000 ) ) ;
#1916 = FACE_OUTER_BOUND ( 'NONE', #1217, .T. ) ;
#1917 = LINE ( 'NONE', #1868, #4763 ) ;
#1918 = ORIENTED_EDGE ( 'NONE', *, *, #2276, .F. ) ;
#1919 = AXIS2_PLACEMENT_3D ( 'NONE', #1036, #2038, #5226 ) ;
#1920 = DIRECTION ( 'NONE',  ( 1.000000000000000000, 0.000000000000000000, 0.000000000000000000 ) ) ;
#1921 = DIRECTION ( 'NONE',  ( 0.000000000000000000, 0.000000000000000000, -1.000000000000000000 ) ) ;
#1922 = AXIS2_PLACEMENT_3D ( 'NONE', #2652, #2830, #464 ) ;
#1923 = CARTESIAN_POINT ( 'NONE',  ( -45.00000000000001421, 40.00000000000000000, -45.00000000000000000 ) ) ;
#1924 = DIRECTION ( 'NONE',  ( 0.000000000000000000, 0.000000000000000000, -1.000000000000000000 ) ) ;
#1925 = EDGE_CURVE ( 'NONE', #2057, #2395, #4212, .T. ) ;
#1926 = VERTEX_POINT ( 'NONE', #2352 ) ;
#1928 = ORIENTED_EDGE ( 'NONE', *, *, #4724, .T. ) ;
#1927 = PRODUCT ( 'clamp', 'clamp', '', ( #596 ) ) ;
#1929 =( NAMED_UNIT ( * ) SI_UNIT ( $, .STERADIAN. ) SOLID_ANGLE_UNIT ( ) );
#1930 = CONICAL_SURFACE ( 'NONE', #5337, 2.500000000000002220, 1.029744260000002631 ) ;
#1931 = FACE_BOUND ( 'NONE', #1104, .T. ) ;
#1932 = ADVANCED_FACE ( 'NONE', ( #1864, #5121, #5097 ), #2778, .T. ) ;
#1933 = AXIS2_PLACEMENT_3D ( 'NONE', #986, #2808, #4699 ) ;
#1934 = ORIENTED_EDGE ( 'NONE', *, *, #4765, .T. ) ;
#1935 = PLANE ( 'NONE',  #1473 ) ;
#1936 = DIRECTION ( 'NONE',  ( -1.000000000000000000, -0.000000000000000000, -0.000000000000000000 ) ) ;
#1937 = VECTOR ( 'NONE', #1951, 1000.000000000000000 ) ;
#1938 = VECTOR ( 'NONE', #4143, 1000.000000000000114 ) ;
#1939 = DIRECTION ( 'NONE',  ( -1.000000000000000000, -0.000000000000000000, -0.000000000000000000 ) ) ;
#1940 = EDGE_CURVE ( 'NONE', #1480, #5831, #5047, .T. ) ;
#1941 = CIRCLE ( 'NONE', #1758, 7.000000000000000000 ) ;
#1942 = ORIENTED_EDGE ( 'NONE', *, *, #2000, .T. ) ;
#1943 = CIRCLE ( 'NONE', #1173, 2.649999999999999467 ) ;
#1944 = ORIENTED_EDGE ( 'NONE', *, *, #994, .T. ) ;
#1945 = CIRCLE ( 'NONE', #892, 7.500000000000000000 ) ;
#1946 = VECTOR ( 'NONE', #4404, 1000.000000000000000 ) ;
#1947 = CARTESIAN_POINT ( 'NONE',  ( 150.0000000000000284, 15.00000000000000000, -45.00000000000000000 ) ) ;
#1948 = ORIENTED_EDGE ( 'NONE', *, *, #5131, .F. ) ;
#1949 = LINE ( 'NONE', #5203, #3492 ) ;
#1950 = LINE ( 'NONE', #2895, #888 ) ;
#1951 = DIRECTION ( 'NONE',  ( 0.000000000000000000, 0.000000000000000000, -1.000000000000000000 ) ) ;
#1952 = ORIENTED_EDGE ( 'NONE', *, *, #280, .F. ) ;
#1953 = PRESENTATION_LAYER_ASSIGNMENT (  '', '', ( #1863 ) ) ;
#1954 = DIRECTION ( 'NONE',  ( 1.000000000000000000, 0.000000000000000000, 0.000000000000000000 ) ) ;
#1955 = CARTESIAN_POINT ( 'NONE',  ( 0.9586399445693630783, 0.5150000000000030109, -0.8293189044373061591 ) ) ;
#1956 = MECHANICAL_DESIGN_GEOMETRIC_PRESENTATION_REPRESENTATION (  '', ( #1185 ), #4684 ) ;
#1957 = LINE ( 'NONE', #2415, #4468 ) ;
#1958 = DIRECTION ( 'NONE',  ( -0.000000000000000000, 1.000000000000000000, 1.224646799147353207E-16 ) ) ;
#1959 = LINE ( 'NONE', #2848, #604 ) ;
#1960 = EDGE_LOOP ( 'NONE', ( #447, #5955, #2287, #2361, #2096, #4038, #4925, #3541, #1537, #2616, #4884, #1196 ) ) ;
#1961 = AXIS2_PLACEMENT_3D ( 'NONE', #930, #5, #5102 ) ;
#1962 = VERTEX_POINT ( 'NONE', #901 ) ;
#1963 = CIRCLE ( 'NONE', #5086, 2.649999999999999467 ) ;
#1964 = CARTESIAN_POINT ( 'NONE',  ( 137.4999999999999716, -15.00000000000000000, 75.00000000000001421 ) ) ;
#1965 = UNCERTAINTY_MEASURE_WITH_UNIT (LENGTH_MEASURE( 1.000000000000000082E-05 ), #2755, 'distance_accuracy_value', 'NONE');
#1966 = ORIENTED_EDGE ( 'NONE', *, *, #1097, .F. ) ;
#1967 = DIRECTION ( 'NONE',  ( 0.000000000000000000, 0.000000000000000000, 1.000000000000000000 ) ) ;
#1968 = ADVANCED_FACE ( 'NONE', ( #2756, #4612 ), #449, .F. ) ;
#1969 = LINE ( 'NONE', #4804, #1977 ) ;
#1970 = ADVANCED_FACE ( 'NONE', ( #621 ), #2466, .T. ) ;
#1971 = DIRECTION ( 'NONE',  ( -0.000000000000000000, -0.000000000000000000, 1.000000000000000000 ) ) ;
#1972 = CARTESIAN_POINT ( 'NONE',  ( -40.66987298107780902, 45.00000000000000000, 52.49999999999999289 ) ) ;
#1974 = VERTEX_POINT ( 'NONE', #4811 ) ;
#1973 = EDGE_CURVE ( 'NONE', #4267, #107, #5683, .T. ) ;
#1975 = ORIENTED_EDGE ( 'NONE', *, *, #5356, .T. ) ;
#1976 = SURFACE_STYLE_USAGE ( .BOTH. , #1125 ) ;
#1977 = VECTOR ( 'NONE', #4715, 1000.000000000000114 ) ;
#1978 = CARTESIAN_POINT ( 'NONE',  ( 75.00000000000001421, 0.000000000000000000, 0.000000000000000000 ) ) ;
#1979 = EDGE_LOOP ( 'NONE', ( #5834, #4788, #2682, #2573, #4041, #5413, #1784, #2694 ) ) ;
#1980 = CARTESIAN_POINT ( 'NONE',  ( 75.00000000000001421, 0.000000000000000000, 9.500000000000000000 ) ) ;
#1981 = CARTESIAN_POINT ( 'NONE',  ( 37.50000000000000711, 6.288372600415927295E-15, -65.00000000000000000 ) ) ;
#1982 = FACE_OUTER_BOUND ( 'NONE', #3729, .T. ) ;
#1983 = VERTEX_POINT ( 'NONE', #142 ) ;
#1984 = DIRECTION ( 'NONE',  ( 6.123233995736766036E-17, 0.000000000000000000, -1.000000000000000000 ) ) ;
#1985 = EDGE_CURVE ( 'NONE', #4600, #2954, #2800, .T. ) ;
#1986 = DIRECTION ( 'NONE',  ( -1.000000000000000000, -0.000000000000000000, -0.000000000000000000 ) ) ;
#1987 = DIRECTION ( 'NONE',  ( 1.000000000000000000, 0.000000000000000000, 0.000000000000000000 ) ) ;
#1988 = DIRECTION ( 'NONE',  ( 1.000000000000000000, 0.000000000000000000, 0.000000000000000000 ) ) ;
#1989 = CARTESIAN_POINT ( 'NONE',  ( 0.3608130681495591019, 0.2499999999999982792, -1.888070236890895703 ) ) ;
#1990 = CARTESIAN_POINT ( 'NONE',  ( 77.00000000000001421, 0.000000000000000000, 9.500000000000000000 ) ) ;
#1991 = ORIENTED_EDGE ( 'NONE', *, *, #5517, .T. ) ;
#1992 = EDGE_LOOP ( 'NONE', ( #3694, #4300, #1510 ) ) ;
#1993 = VECTOR ( 'NONE', #3837, 1000.000000000000000 ) ;
#1994 = CYLINDRICAL_SURFACE ( 'NONE', #5653, 5.000000000000000000 ) ;
#1995 = ORIENTED_EDGE ( 'NONE', *, *, #2425, .T. ) ;
#1996 = DIRECTION ( 'NONE',  ( -1.000000000000000000, -0.000000000000000000, -0.000000000000000000 ) ) ;
#1997 = DIRECTION ( 'NONE',  ( -1.000000000000000000, 0.000000000000000000, 0.000000000000000000 ) ) ;
#1998 = CARTESIAN_POINT ( 'NONE',  ( 137.4999999999999716, 0.000000000000000000, 0.000000000000000000 ) ) ;
#1999 = DIRECTION ( 'NONE',  ( -0.000000000000000000, -1.000000000000000000, -0.000000000000000000 ) ) ;
#2000 = EDGE_CURVE ( 'NONE', #1524, #3408, #2315, .T. ) ;
#2001 = ORIENTED_EDGE ( 'NONE', *, *, #5660, .F. ) ;
#2002 = ADVANCED_FACE ( 'NONE', ( #3470 ), #4782, .F. ) ;
#2003 = VERTEX_POINT ( 'NONE', #4329 ) ;
#2004 = LINE ( 'NONE', #1590, #3295 ) ;
#2005 = EDGE_CURVE ( 'NONE', #225, #4357, #1127, .T. ) ;
#2006 = CARTESIAN_POINT ( 'NONE',  ( 37.50000000000000711, 6.288372600415927295E-15, -65.00000000000000000 ) ) ;
#2007 = ORIENTED_EDGE ( 'NONE', *, *, #2699, .T. ) ;
#2008 = PLANE ( 'NONE',  #1657 ) ;
#2009 = FACE_BOUND ( 'NONE', #2470, .T. ) ;
#2010 = CARTESIAN_POINT ( 'NONE',  ( 75.00000000000001421, 0.000000000000000000, -9.500000000000000000 ) ) ;
#2011 = EDGE_LOOP ( 'NONE', ( #5869, #5688, #1358, #5895 ) ) ;
#2012 = DIRECTION ( 'NONE',  ( -1.000000000000000000, 0.000000000000000000, 0.000000000000000000 ) ) ;
#2013 = CARTESIAN_POINT ( 'NONE',  ( -40.66987298107781612, 45.00000000000000000, 37.50000000000000000 ) ) ;
#2014 = FACE_BOUND ( 'NONE', #796, .T. ) ;
#2015 = PLANE ( 'NONE',  #676 ) ;
#2016 = FACE_OUTER_BOUND ( 'NONE', #4826, .T. ) ;
#2017 = DIRECTION ( 'NONE',  ( 0.000000000000000000, 1.000000000000000000, 0.000000000000000000 ) ) ;
#2018 = AXIS2_PLACEMENT_3D ( 'NONE', #1100, #4356, #3146 ) ;
#2019 = EDGE_CURVE ( 'NONE', #3083, #342, #3097, .T. ) ;
#2020 = CIRCLE ( 'NONE', #2212, 4.999999999999990230 ) ;
#2021 = EDGE_LOOP ( 'NONE', ( #3936, #1667, #5852, #3510 ) ) ;
#2022 = CYLINDRICAL_SURFACE ( 'NONE', #1207, 5.499999999999991118 ) ;
#2023 =( NAMED_UNIT ( * ) SI_UNIT ( $, .STERADIAN. ) SOLID_ANGLE_UNIT ( ) );
#2024 = APPLICATION_CONTEXT ( 'automotive_design' ) ;
#2025 = CARTESIAN_POINT ( 'NONE',  ( 2.740000000000000213, -0.6774776749089226335, -0.5150000000000000133 ) ) ;
#2026 = UNCERTAINTY_MEASURE_WITH_UNIT (LENGTH_MEASURE( 1.000000000000000082E-05 ), #2116, 'distance_accuracy_value', 'NONE');
#2027 =( GEOMETRIC_REPRESENTATION_CONTEXT ( 3 ) GLOBAL_UNCERTAINTY_ASSIGNED_CONTEXT ( ( #157 ) ) GLOBAL_UNIT_ASSIGNED_CONTEXT ( ( #285, #1772, #4074 ) ) REPRESENTATION_CONTEXT ( 'NONE', 'WORKASPACE' ) );
#2028 = VERTEX_POINT ( 'NONE', #4876 ) ;
#2029 = CIRCLE ( 'NONE', #3584, 4.749999999999999112 ) ;
#2030 = FACE_OUTER_BOUND ( 'NONE', #2819, .T. ) ;
#2031 = CONICAL_SURFACE ( 'NONE', #1549, 2.500000000000002220, 1.029744260000002631 ) ;
#2032 = CARTESIAN_POINT ( 'NONE',  ( 75.00000000000001421, 0.000000000000000000, -7.000000000000000000 ) ) ;
#2033 = ORIENTED_EDGE ( 'NONE', *, *, #4675, .F. ) ;
#2034 = ORIENTED_EDGE ( 'NONE', *, *, #2195, .F. ) ;
#2035 = AXIS2_PLACEMENT_3D ( 'NONE', #4550, #2632, #393 ) ;
#2036 = CIRCLE ( 'NONE', #4274, 5.499999999999998224 ) ;
#2037 = SURFACE_STYLE_FILL_AREA ( #2956 ) ;
#2038 = DIRECTION ( 'NONE',  ( -1.000000000000000000, -0.000000000000000000, -0.000000000000000000 ) ) ;
#2039 = EDGE_LOOP ( 'NONE', ( #3911, #4544, #5055, #4116 ) ) ;
#2040 = AXIS2_PLACEMENT_3D ( 'NONE', #5893, #1740, #4045 ) ;
#2041 = CIRCLE ( 'NONE', #3596, 2.500000000000002220 ) ;
#2042 = CARTESIAN_POINT ( 'NONE',  ( -36.33974596215562514, 40.00000000000000000, 44.99999999999999289 ) ) ;
#2043 = CARTESIAN_POINT ( 'NONE',  ( -36.33974596215562514, 45.00000000000000000, 44.99999999999999289 ) ) ;
#2044 = DIRECTION ( 'NONE',  ( 0.000000000000000000, 0.000000000000000000, -1.000000000000000000 ) ) ;
#2045 = VERTEX_POINT ( 'NONE', #2957 ) ;
#2046 = AXIS2_PLACEMENT_3D ( 'NONE', #2203, #300, #4052 ) ;
#2047 = CARTESIAN_POINT ( 'NONE',  ( 78.30000000000002558, 0.000000000000000000, 9.499999999999994671 ) ) ;
#2048 = CIRCLE ( 'NONE', #697, 7.000000000000000000 ) ;
#2049 = CARTESIAN_POINT ( 'NONE',  ( 25.00000000000000711, -6.999999999999988454, 65.00000000000000000 ) ) ;
#2050 = EDGE_CURVE ( 'NONE', #2958, #1875, #3384, .T. ) ;
#2051 = CARTESIAN_POINT ( 'NONE',  ( 1.849560077140140812, 0.5149999999999973488, 0.7556913915602433418 ) ) ;
#2052 = DIRECTION ( 'NONE',  ( -0.5000000000000003331, 0.000000000000000000, -0.8660254037844383745 ) ) ;
#2053 = CARTESIAN_POINT ( 'NONE',  ( -45.00000000000001421, 50.00000000000000000, 45.00000000000000000 ) ) ;
#2054 =( GEOMETRIC_REPRESENTATION_CONTEXT ( 3 ) GLOBAL_UNCERTAINTY_ASSIGNED_CONTEXT ( ( #1607 ) ) GLOBAL_UNIT_ASSIGNED_CONTEXT ( ( #5602, #608, #1929 ) ) REPRESENTATION_CONTEXT ( 'NONE', 'WORKASPACE' ) );
#2056 = VECTOR ( 'NONE', #4989, 1000.000000000000000 ) ;
#2055 = CARTESIAN_POINT ( 'NONE',  ( -55.00000000000001421, 30.00000000000000355, 45.00000000000000000 ) ) ;
#2057 = VERTEX_POINT ( 'NONE', #712 ) ;
#2058 = EDGE_CURVE ( 'NONE', #5304, #1524, #2557, .T. ) ;
#2059 = VERTEX_POINT ( 'NONE', #4419 ) ;
#2060 = FILL_AREA_STYLE_COLOUR ( '', #2747 ) ;
#2061 = CARTESIAN_POINT ( 'NONE',  ( 0.000000000000000000, 0.000000000000000000, 0.000000000000000000 ) ) ;
#2062 = ADVANCED_FACE ( 'NONE', ( #3377 ), #2099, .F. ) ;
#2063 = VERTEX_POINT ( 'NONE', #1065 ) ;
#2064 = LINE ( 'NONE', #5531, #3982 ) ;
#2065 = FILL_AREA_STYLE ('',( #4378 ) ) ;
#2066 = DIRECTION ( 'NONE',  ( 1.000000000000000000, 0.000000000000000000, 0.000000000000000000 ) ) ;
#2067 = EDGE_CURVE ( 'NONE', #4142, #1478, #4837, .T. ) ;
#2068 = CIRCLE ( 'NONE', #2945, 5.000000000000004441 ) ;
#2069 = CARTESIAN_POINT ( 'NONE',  ( 65.15000000000001990, -1.951563910473909559E-15, 71.29999999999999716 ) ) ;
#2070 = ORIENTED_EDGE ( 'NONE', *, *, #2916, .T. ) ;
#2071 = EDGE_LOOP ( 'NONE', ( #351, #3448 ) ) ;
#2072 = CARTESIAN_POINT ( 'NONE',  ( -45.00000000000002842, 15.00000000000000000, -44.99999999999998579 ) ) ;
#2073 = CARTESIAN_POINT ( 'NONE',  ( 1.299999999999999600, 1.000000000000000000, 0.000000000000000000 ) ) ;
#2074 = ORIENTED_EDGE ( 'NONE', *, *, #1465, .T. ) ;
#2075 = FACE_BOUND ( 'NONE', #3051, .T. ) ;
#2076 = DIRECTION ( 'NONE',  ( -0.000000000000000000, -1.000000000000000000, -0.000000000000000000 ) ) ;
#2077 = VECTOR ( 'NONE', #3878, 1000.000000000000000 ) ;
#2078 = CYLINDRICAL_SURFACE ( 'NONE', #5919, 0.9999999999999991118 ) ;
#2079 = VERTEX_POINT ( 'NONE', #5745 ) ;
#2080 = PRODUCT_CONTEXT ( 'NONE', #5443, 'mechanical' ) ;
#2081 = DIRECTION ( 'NONE',  ( 0.000000000000000000, 0.000000000000000000, -1.000000000000000000 ) ) ;
#2082 = FACE_BOUND ( 'NONE', #2783, .T. ) ;
#2083 = DIRECTION ( 'NONE',  ( 0.000000000000000000, 0.000000000000000000, 1.000000000000000000 ) ) ;
#2084 = CARTESIAN_POINT ( 'NONE',  ( 0.000000000000000000, 0.5150000000000083400, -2.349999999999997424 ) ) ;
#2085 = DIRECTION ( 'NONE',  ( 0.000000000000000000, 1.000000000000000000, 0.000000000000000000 ) ) ;
#2086 = EDGE_CURVE ( 'NONE', #4227, #3393, #1246, .T. ) ;
#2087 = ORIENTED_EDGE ( 'NONE', *, *, #4093, .F. ) ;
#2088 = EDGE_CURVE ( 'NONE', #4783, #4354, #5708, .T. ) ;
#2089 = ORIENTED_EDGE ( 'NONE', *, *, #1610, .T. ) ;
#2090 = CARTESIAN_POINT ( 'NONE',  ( 25.00000000000000711, -6.999999999999988454, -65.00000000000000000 ) ) ;
#2091 = PRODUCT_DEFINITION_CONTEXT ( 'detailed design', #555, 'design' ) ;
#2092 = EDGE_CURVE ( 'NONE', #2669, #4799, #865, .T. ) ;
#2093 = ORIENTED_EDGE ( 'NONE', *, *, #2645, .F. ) ;
#2094 = LINE ( 'NONE', #732, #5600 ) ;
#2095 = CARTESIAN_POINT ( 'NONE',  ( 1.849560077140107950, -0.5150000000000023448, 0.7556913915602430087 ) ) ;
#2096 = ORIENTED_EDGE ( 'NONE', *, *, #3225, .F. ) ;
#2097 = ADVANCED_FACE ( 'NONE', ( #5267 ), #4748, .T. ) ;
#2098 = EDGE_LOOP ( 'NONE', ( #3653, #1247, #495, #4762 ) ) ;
#2099 = CYLINDRICAL_SURFACE ( 'NONE', #3855, 5.499999999999991118 ) ;
#2100 = ORIENTED_EDGE ( 'NONE', *, *, #3397, .F. ) ;
#2101 = DIRECTION ( 'NONE',  ( 0.000000000000000000, 0.000000000000000000, 1.000000000000000000 ) ) ;
#2102 = CARTESIAN_POINT ( 'NONE',  ( -25.39999999999996305, 1.224646799147353207E-16, -1.000000000000000000 ) ) ;
#2103 =( REPRESENTATION_RELATIONSHIP ('NONE','NONE', #5609, #2622 ) REPRESENTATION_RELATIONSHIP_WITH_TRANSFORMATION ( #5259 )SHAPE_REPRESENTATION_RELATIONSHIP( ) );
#2104 = DIRECTION ( 'NONE',  ( -0.000000000000000000, -0.000000000000000000, -1.000000000000000000 ) ) ;
#2105 = EDGE_LOOP ( 'NONE', ( #918, #67, #158, #3993, #3382, #4734 ) ) ;
#2106 =( NAMED_UNIT ( * ) SI_UNIT ( $, .STERADIAN. ) SOLID_ANGLE_UNIT ( ) );
#2107 = CARTESIAN_POINT ( 'NONE',  ( 2.740000000000000213, 0.000000000000000000, 0.000000000000000000 ) ) ;
#2108 = AXIS2_PLACEMENT_3D ( 'NONE', #2629, #866, #5071 ) ;
#2109 = DIRECTION ( 'NONE',  ( -1.000000000000000000, 0.000000000000000000, -0.000000000000000000 ) ) ;
#2110 = FACE_OUTER_BOUND ( 'NONE', #5956, .T. ) ;
#2111 = FACE_BOUND ( 'NONE', #3656, .T. ) ;
#2112 = LINE ( 'NONE', #3933, #5934 ) ;
#2113 = ORIENTED_EDGE ( 'NONE', *, *, #3287, .T. ) ;
#2114 = AXIS2_PLACEMENT_3D ( 'NONE', #1294, #2201, #2268 ) ;
#2115 = EDGE_LOOP ( 'NONE', ( #586, #5648, #3626, #4710, #3081, #5244, #5587, #5254, #3632, #4766, #4070, #816 ) ) ;
#2116 =( LENGTH_UNIT ( ) NAMED_UNIT ( * ) SI_UNIT ( .MILLI., .METRE. ) );
#2117 = AXIS2_PLACEMENT_3D ( 'NONE', #3634, #840, #2175 ) ;
#2118 = CARTESIAN_POINT ( 'NONE',  ( -45.00000000000001421, 45.00000000000000000, 50.00000000000000000 ) ) ;
#2119 = EDGE_LOOP ( 'NONE', ( #2199, #81, #1911, #2835, #2730, #4075, #4394, #2291 ) ) ;
#2120 = EDGE_CURVE ( 'NONE', #2598, #4174, #2215, .T. ) ;
#2121 =( NAMED_UNIT ( * ) SI_UNIT ( $, .STERADIAN. ) SOLID_ANGLE_UNIT ( ) );
#2122 = PRODUCT_RELATED_PRODUCT_CATEGORY ( 'part', '', ( #5230 ) ) ;
#2123 = VECTOR ( 'NONE', #170, 1000.000000000000000 ) ;
#2124 = CARTESIAN_POINT ( 'NONE',  ( 55.00000000000000711, 8.572527594031473190E-16, 7.000000000000000000 ) ) ;
#2125 = CARTESIAN_POINT ( 'NONE',  ( -45.00000000000001421, 0.000000000000000000, 39.99999999999999289 ) ) ;
#2126 = VERTEX_POINT ( 'NONE', #325 ) ;
#2127 = ORIENTED_EDGE ( 'NONE', *, *, #3252, .F. ) ;
#2128 = VECTOR ( 'NONE', #4918, 1000.000000000000000 ) ;
#2129 = EDGE_CURVE ( 'NONE', #4498, #94, #5409, .T. ) ;
#2130 = ORIENTED_EDGE ( 'NONE', *, *, #5761, .T. ) ;
#2131 = CARTESIAN_POINT ( 'NONE',  ( 3.699999999999998401, 0.000000000000000000, 0.000000000000000000 ) ) ;
#2132 = CARTESIAN_POINT ( 'NONE',  ( 9.300000000000002487, 1.224646799147353207E-16, -1.000000000000000000 ) ) ;
#2133 = ORIENTED_EDGE ( 'NONE', *, *, #2548, .T. ) ;
#2134 = DIRECTION ( 'NONE',  ( 0.000000000000000000, 1.000000000000000000, 0.000000000000000000 ) ) ;
#2135 = AXIS2_PLACEMENT_3D ( 'NONE', #3768, #952, #1014 ) ;
#2136 = ORIENTED_EDGE ( 'NONE', *, *, #1383, .F. ) ;
#2137 = CARTESIAN_POINT ( 'NONE',  ( -25.39999999999996305, 0.000000000000000000, 0.000000000000000000 ) ) ;
#2138 = VECTOR ( 'NONE', #116, 1000.000000000000000 ) ;
#2139 = VECTOR ( 'NONE', #3110, 1000.000000000000000 ) ;
#2140 = DIRECTION ( 'NONE',  ( 0.000000000000000000, 1.000000000000000000, 0.000000000000000000 ) ) ;
#2141 = LINE ( 'NONE', #4821, #2128 ) ;
#2142 = FACE_OUTER_BOUND ( 'NONE', #1251, .T. ) ;
#2143 = CARTESIAN_POINT ( 'NONE',  ( -55.00000000000001421, 40.00000000000000000, -45.00000000000000000 ) ) ;
#2144 = ORIENTED_EDGE ( 'NONE', *, *, #4737, .F. ) ;
#2145 = AXIS2_PLACEMENT_3D ( 'NONE', #3151, #3509, #5868 ) ;
#2146 = AXIS2_PLACEMENT_3D ( 'NONE', #1340, #895, #974 ) ;
#2147 =( NAMED_UNIT ( * ) SI_UNIT ( $, .STERADIAN. ) SOLID_ANGLE_UNIT ( ) );
#2148 = CARTESIAN_POINT ( 'NONE',  ( -25.39999999999996305, 0.000000000000000000, 0.000000000000000000 ) ) ;
#2149 = AXIS2_PLACEMENT_3D ( 'NONE', #4002, #5456, #3158 ) ;
#2150 = AXIS2_PLACEMENT_3D ( 'NONE', #1095, #552, #165 ) ;
#2151 = EDGE_LOOP ( 'NONE', ( #998, #1254, #357, #5562 ) ) ;
#2152 = CARTESIAN_POINT ( 'NONE',  ( -25.39999999999996305, 0.000000000000000000, 4.749999999999999112 ) ) ;
#2153 = AXIS2_PLACEMENT_3D ( 'NONE', #916, #5500, #1796 ) ;
#2154 = COLOUR_RGB ( '',0.8941176470588234615, 0.8941176470588234615, 0.8941176470588234615 ) ;
#2155 =( LENGTH_UNIT ( ) NAMED_UNIT ( * ) SI_UNIT ( .MILLI., .METRE. ) );
#2156 = DIRECTION ( 'NONE',  ( 0.000000000000000000, 0.000000000000000000, -1.000000000000000000 ) ) ;
#2157 = CARTESIAN_POINT ( 'NONE',  ( 2.740000000000000213, -0.6774776749089226335, -0.5150000000000000133 ) ) ;
#2158 = MECHANICAL_DESIGN_GEOMETRIC_PRESENTATION_REPRESENTATION (  '', ( #4298 ), #3326 ) ;
#2159 = VERTEX_POINT ( 'NONE', #1250 ) ;
#2160 = EDGE_CURVE ( 'NONE', #2555, #635, #3077, .T. ) ;
#2161 = EDGE_LOOP ( 'NONE', ( #1282, #290, #5181 ) ) ;
#2162 = EDGE_CURVE ( 'NONE', #5475, #1708, #801, .T. ) ;
#2163 = FILL_AREA_STYLE_COLOUR ( '', #3985 ) ;
#2164 = PRODUCT_DEFINITION_FORMATION_WITH_SPECIFIED_SOURCE ( 'ANY', '', #494, .NOT_KNOWN. ) ;
#2165 = CARTESIAN_POINT ( 'NONE',  ( 37.50000000000000711, 6.288372600415927295E-15, 65.00000000000000000 ) ) ;
#2166 = ORIENTED_EDGE ( 'NONE', *, *, #4514, .F. ) ;
#2167 = EDGE_CURVE ( 'NONE', #1426, #5354, #574, .T. ) ;
#2168 = CARTESIAN_POINT ( 'NONE',  ( 59.85000000000001563, -1.627032508699861061E-15, 71.29999999999999716 ) ) ;
#2169 = CARTESIAN_POINT ( 'NONE',  ( -45.00000000000001421, 28.00000000000000355, 50.00000000000000000 ) ) ;
#2170 = EDGE_LOOP ( 'NONE', ( #4031, #5677, #4572, #2136 ) ) ;
#2171 = LINE ( 'NONE', #4021, #1460 ) ;
#2172 = ORIENTED_EDGE ( 'NONE', *, *, #1082, .T. ) ;
#2173 = CONTEXT_DEPENDENT_SHAPE_REPRESENTATION ( #3464, #5666 ) ;
#2174 = DIRECTION ( 'NONE',  ( 0.000000000000000000, 0.000000000000000000, 1.000000000000000000 ) ) ;
#2175 = DIRECTION ( 'NONE',  ( 0.000000000000000000, 0.000000000000000000, 1.000000000000000000 ) ) ;
#2176 = CARTESIAN_POINT ( 'NONE',  ( 0.06760930072668894231, 0.9010842325122832008, -0.5150000000000000133 ) ) ;
#2177 = LINE ( 'NONE', #5042, #4969 ) ;
#2178 = DIRECTION ( 'NONE',  ( -0.000000000000000000, -0.000000000000000000, -1.000000000000000000 ) ) ;
#2179 = ORIENTED_EDGE ( 'NONE', *, *, #2796, .T. ) ;
#2180 = EDGE_CURVE ( 'NONE', #3717, #542, #4016, .T. ) ;
#2181 = CARTESIAN_POINT ( 'NONE',  ( 0.9586399445693771781, -0.8293189044373066032, -0.5150000000000000133 ) ) ;
#2182 = MANIFOLD_SOLID_BREP ( 'Boss-Extrude1', #147 ) ;
#2183 = EDGE_LOOP ( 'NONE', ( #3761, #5439, #4702, #1966 ) ) ;
#2184 = CARTESIAN_POINT ( 'NONE',  ( 2.740000000000000213, 0.9838866223910001096, -0.5150000000000001243 ) ) ;
#2185 =( NAMED_UNIT ( * ) PLANE_ANGLE_UNIT ( ) SI_UNIT ( $, .RADIAN. ) );
#2186 = DIRECTION ( 'NONE',  ( 1.000000000000000000, 0.000000000000000000, 0.000000000000000000 ) ) ;
#2187 = DIRECTION ( 'NONE',  ( -0.000000000000000000, -0.000000000000000000, -1.000000000000000000 ) ) ;
#2188 = ORIENTED_EDGE ( 'NONE', *, *, #611, .F. ) ;
#2189 = MANIFOLD_SOLID_BREP ( 'Cavity1', #1878 ) ;
#2190 = ORIENTED_EDGE ( 'NONE', *, *, #5483, .T. ) ;
#2191 = VECTOR ( 'NONE', #628, 1000.000000000000000 ) ;
#2192 = ORIENTED_EDGE ( 'NONE', *, *, #2465, .T. ) ;
#2193 = DIRECTION ( 'NONE',  ( 0.000000000000000000, 0.000000000000000000, 1.000000000000000000 ) ) ;
#2194 = FACE_OUTER_BOUND ( 'NONE', #2313, .T. ) ;
#2195 = EDGE_CURVE ( 'NONE', #5283, #1741, #3175, .T. ) ;
#2196 = CIRCLE ( 'NONE', #4926, 2.500000000000000000 ) ;
#2197 = VERTEX_POINT ( 'NONE', #3108 ) ;
#2198 = DIRECTION ( 'NONE',  ( -1.000000000000000000, 0.000000000000000000, 0.000000000000000000 ) ) ;
#2199 = ORIENTED_EDGE ( 'NONE', *, *, #2906, .F. ) ;
#2200 = ADVANCED_FACE ( 'NONE', ( #855 ), #2258, .F. ) ;
#2201 = DIRECTION ( 'NONE',  ( 0.4461977533474923430, 3.124646727056501017E-15, -0.8949343913984144638 ) ) ;
#2202 = CARTESIAN_POINT ( 'NONE',  ( 67.00000000000000000, 1.224646799147354440E-16, -8.500000000000000000 ) ) ;
#2203 = CARTESIAN_POINT ( 'NONE',  ( -25.39999999999996305, 0.000000000000000000, 0.000000000000000000 ) ) ;
#2204 = DIRECTION ( 'NONE',  ( 0.000000000000000000, 0.000000000000000000, 1.000000000000000000 ) ) ;
#2205 = ORIENTED_EDGE ( 'NONE', *, *, #1451, .F. ) ;
#2206 = PRESENTATION_STYLE_ASSIGNMENT (( #1237 ) ) ;
#2207 = LINE ( 'NONE', #1755, #2453 ) ;
#2208 = EDGE_CURVE ( 'NONE', #5930, #554, #5332, .T. ) ;
#2209 = MANIFOLD_SOLID_BREP ( 'Boss-Extrude2', #2762 ) ;
#2210 = ORIENTED_EDGE ( 'NONE', *, *, #751, .F. ) ;
#2211 = DIRECTION ( 'NONE',  ( 0.000000000000000000, 0.000000000000000000, 1.000000000000000000 ) ) ;
#2212 = AXIS2_PLACEMENT_3D ( 'NONE', #3528, #4929, #5857 ) ;
#2213 = CARTESIAN_POINT ( 'NONE',  ( 150.0000000000000284, 0.000000000000000000, 45.00000000000000000 ) ) ;
#2214 = EDGE_LOOP ( 'NONE', ( #862, #5421, #633, #4556 ) ) ;
#2215 = CIRCLE ( 'NONE', #5605, 0.8509999999999999787 ) ;
#2216 = ORIENTED_EDGE ( 'NONE', *, *, #5552, .T. ) ;
#2217 = DIRECTION ( 'NONE',  ( 0.000000000000000000, 0.000000000000000000, 1.000000000000000000 ) ) ;
#2218 = VECTOR ( 'NONE', #3284, 1000.000000000000000 ) ;
#2219 = ORIENTED_EDGE ( 'NONE', *, *, #3575, .T. ) ;
#2220 = VECTOR ( 'NONE', #4442, 1000.000000000000227 ) ;
#2221 = LINE ( 'NONE', #355, #2139 ) ;
#2222 = DIRECTION ( 'NONE',  ( 0.000000000000000000, 0.000000000000000000, -1.000000000000000000 ) ) ;
#2223 = ORIENTED_EDGE ( 'NONE', *, *, #2394, .T. ) ;
#2224 = CARTESIAN_POINT ( 'NONE',  ( 75.00000000000001421, 8.572527594031473190E-16, 7.000000000000000000 ) ) ;
#2225 = COLOUR_RGB ( '',1.000000000000000000, 0.9490196078431372140, 0.9098039215686274384 ) ;
#2226 = EDGE_LOOP ( 'NONE', ( #852, #1310, #3329, #3767 ) ) ;
#2227 = CIRCLE ( 'NONE', #2423, 12.00000000000000000 ) ;
#2228 = VERTEX_POINT ( 'NONE', #1459 ) ;
#2229 = DIRECTION ( 'NONE',  ( 0.000000000000000000, 0.000000000000000000, 1.000000000000000000 ) ) ;
#2230 = MECHANICAL_DESIGN_GEOMETRIC_PRESENTATION_REPRESENTATION (  '', ( #4660 ), #4072 ) ;
#2231 = CARTESIAN_POINT ( 'NONE',  ( 0.06760930072668813740, -0.5150000000000026779, 0.9010842325122891960 ) ) ;
#2232 = CARTESIAN_POINT ( 'NONE',  ( 67.00000000000001421, 0.000000000000000000, 0.000000000000000000 ) ) ;
#2233 = CARTESIAN_POINT ( 'NONE',  ( 24.99999999999998224, -7.000000000000006217, 65.00000000000000000 ) ) ;
#2234 = PRODUCT ( 'movable block', 'movable block', '', ( #3928 ) ) ;
#2235 = EDGE_LOOP ( 'NONE', ( #1912, #1733, #2549, #2365 ) ) ;
#2236 = EDGE_CURVE ( 'NONE', #2685, #5415, #75, .T. ) ;
#2237 = CIRCLE ( 'NONE', #3780, 1.099999999999998535 ) ;
#2238 = AXIS2_PLACEMENT_3D ( 'NONE', #857, #4569, #3654 ) ;
#2239 = EDGE_CURVE ( 'NONE', #4118, #3289, #5090, .T. ) ;
#2240 = DIRECTION ( 'NONE',  ( 0.000000000000000000, 0.000000000000000000, -1.000000000000000000 ) ) ;
#2241 = ORIENTED_EDGE ( 'NONE', *, *, #4277, .T. ) ;
#2242 = AXIS2_PLACEMENT_3D ( 'NONE', #122, #2540, #4341 ) ;
#2243 = ADVANCED_FACE ( 'NONE', ( #5171 ), #2903, .F. ) ;
#2245 = VECTOR ( 'NONE', #4173, 1000.000000000000000 ) ;
#2244 = CARTESIAN_POINT ( 'NONE',  ( 162.5000000000000000, 15.00000000000000000, 75.00000000000001421 ) ) ;
#2246 =( NAMED_UNIT ( * ) SI_UNIT ( $, .STERADIAN. ) SOLID_ANGLE_UNIT ( ) );
#2247 = FACE_OUTER_BOUND ( 'NONE', #2374, .T. ) ;
#2248 = AXIS2_PLACEMENT_3D ( 'NONE', #3722, #3270, #5123 ) ;
#2249 = VECTOR ( 'NONE', #568, 1000.000000000000000 ) ;
#2250 = FACE_OUTER_BOUND ( 'NONE', #3231, .T. ) ;
#2251 = ORIENTED_EDGE ( 'NONE', *, *, #5010, .F. ) ;
#2252 = CIRCLE ( 'NONE', #5823, 1.037871761867652065 ) ;
#2253 = ORIENTED_EDGE ( 'NONE', *, *, #2566, .F. ) ;
#2254 = EDGE_CURVE ( 'NONE', #2063, #5408, #4362, .T. ) ;
#2255 = FACE_OUTER_BOUND ( 'NONE', #2119, .T. ) ;
#2256 = AXIS2_PLACEMENT_3D ( 'NONE', #4492, #2140, #5847 ) ;
#2257 = MECHANICAL_DESIGN_GEOMETRIC_PRESENTATION_REPRESENTATION (  '', ( #4595 ), #3711 ) ;
#2258 = PLANE ( 'NONE',  #4951 ) ;
#2259 = VERTEX_POINT ( 'NONE', #2771 ) ;
#2260 = CARTESIAN_POINT ( 'NONE',  ( 3.900000000000000799, 0.000000000000000000, 0.000000000000000000 ) ) ;
#2261 = DIRECTION ( 'NONE',  ( -1.000000000000000000, -0.000000000000000000, -0.000000000000000000 ) ) ;
#2262 = ORIENTED_EDGE ( 'NONE', *, *, #135, .F. ) ;
#2263 = CARTESIAN_POINT ( 'NONE',  ( 0.2300425840023382074, 0.2499999999999982236, -1.812072026511089229 ) ) ;
#2264 = VERTEX_POINT ( 'NONE', #4689 ) ;
#2265 = AXIS2_PLACEMENT_3D ( 'NONE', #1438, #4703, #1843 ) ;
#2266 = SURFACE_STYLE_USAGE ( .BOTH. , #4576 ) ;
#2267 = CIRCLE ( 'NONE', #5464, 5.000000000000004441 ) ;
#2268 = DIRECTION ( 'NONE',  ( -0.8949343913984144638, 0.000000000000000000, -0.4461977533474923430 ) ) ;
#2269 = DIRECTION ( 'NONE',  ( -0.4999999999999987232, 0.000000000000000000, 0.8660254037844393737 ) ) ;
#2270 = VECTOR ( 'NONE', #5287, 1000.000000000000000 ) ;
#2271 = DIRECTION ( 'NONE',  ( 1.000000000000000000, 0.000000000000000000, -0.000000000000000000 ) ) ;
#2272 = DIRECTION ( 'NONE',  ( 0.000000000000000000, 1.000000000000000000, 0.000000000000000000 ) ) ;
#2273 = VERTEX_POINT ( 'NONE', #4717 ) ;
#2274 = DIRECTION ( 'NONE',  ( 0.000000000000000000, 0.000000000000000000, -1.000000000000000000 ) ) ;
#2275 = ORIENTED_EDGE ( 'NONE', *, *, #1449, .T. ) ;
#2276 = EDGE_CURVE ( 'NONE', #3852, #5304, #871, .T. ) ;
#2277 = DIRECTION ( 'NONE',  ( 0.000000000000000000, -1.224646799147352714E-16, 1.000000000000000000 ) ) ;
#2278 = EDGE_CURVE ( 'NONE', #1725, #2563, #671, .T. ) ;
#2279 = FACE_OUTER_BOUND ( 'NONE', #5448, .T. ) ;
#2280 = PRODUCT_DEFINITION ( 'UNKNOWN', '', #432, #4919 ) ;
#2281 = DIRECTION ( 'NONE',  ( 1.000000000000000000, -0.000000000000000000, -0.000000000000000000 ) ) ;
#2282 = EDGE_LOOP ( 'NONE', ( #1467, #2674, #3212, #4607 ) ) ;
#2283 = EDGE_LOOP ( 'NONE', ( #5331, #1622, #1619, #4193 ) ) ;
#2284 = CYLINDRICAL_SURFACE ( 'NONE', #4124, 5.000000000000000000 ) ;
#2285 = CONTEXT_DEPENDENT_SHAPE_REPRESENTATION ( #1295, #2370 ) ;
#2286 = DIRECTION ( 'NONE',  ( 0.000000000000000000, 3.656775105596099119E-15, -1.000000000000000000 ) ) ;
#2287 = ORIENTED_EDGE ( 'NONE', *, *, #315, .T. ) ;
#2288 = CARTESIAN_POINT ( 'NONE',  ( 2.740000000000000213, 0.5149999999999976819, 0.6774776749089244099 ) ) ;
#2289 = EDGE_CURVE ( 'NONE', #225, #1034, #4845, .T. ) ;
#2290 = DIRECTION ( 'NONE',  ( 0.000000000000000000, 0.000000000000000000, 1.000000000000000000 ) ) ;
#2291 = ORIENTED_EDGE ( 'NONE', *, *, #2458, .F. ) ;
#2292 = EDGE_LOOP ( 'NONE', ( #41, #2865, #2774 ) ) ;
#2293 = FILL_AREA_STYLE_COLOUR ( '', #297 ) ;
#2294 = CARTESIAN_POINT ( 'NONE',  ( 137.4999999999999716, -6.999999999999985789, -75.00000000000000000 ) ) ;
#2295 = CARTESIAN_POINT ( 'NONE',  ( 24.99999999999998224, -7.000000000000006217, 75.00000000000000000 ) ) ;
#2296 = CARTESIAN_POINT ( 'NONE',  ( 67.00000000000000000, 0.000000000000000000, 9.500000000000000000 ) ) ;
#2297 = DIRECTION ( 'NONE',  ( 0.000000000000000000, 8.673617379884040402E-17, 1.000000000000000000 ) ) ;
#2298 = ORIENTED_EDGE ( 'NONE', *, *, #5438, .F. ) ;
#2299 = CARTESIAN_POINT ( 'NONE',  ( 0.000000000000000000, 0.000000000000000000, 0.000000000000000000 ) ) ;
#2300 = CARTESIAN_POINT ( 'NONE',  ( 2.740000000000000213, 0.000000000000000000, 0.000000000000000000 ) ) ;
#2301 = LINE ( 'NONE', #1046, #34 ) ;
#2302 = ADVANCED_FACE ( 'NONE', ( #2857 ), #484, .F. ) ;
#2303 = CARTESIAN_POINT ( 'NONE',  ( 32.00000000000000711, 6.961928339946972976E-15, 71.29999999999999716 ) ) ;
#2304 = VERTEX_POINT ( 'NONE', #5502 ) ;
#2305 = LINE ( 'NONE', #378, #1862 ) ;
#2306 = APPLICATION_PROTOCOL_DEFINITION ( 'draft international standard', 'automotive_design', 1998, #4520 ) ;
#2307 = EDGE_CURVE ( 'NONE', #1708, #3671, #3581, .T. ) ;
#2308 = CARTESIAN_POINT ( 'NONE',  ( 1.299999999999999156, 0.000000000000000000, 0.000000000000000000 ) ) ;
#2309 = ORIENTED_EDGE ( 'NONE', *, *, #4779, .F. ) ;
#2310 = AXIS2_PLACEMENT_3D ( 'NONE', #4942, #776, #527 ) ;
#2311 = FACE_OUTER_BOUND ( 'NONE', #5227, .T. ) ;
#2312 = VERTEX_POINT ( 'NONE', #4606 ) ;
#2313 = EDGE_LOOP ( 'NONE', ( #3715, #966, #4508, #3808 ) ) ;
#2314 =( NAMED_UNIT ( * ) SI_UNIT ( $, .STERADIAN. ) SOLID_ANGLE_UNIT ( ) );
#2315 = CIRCLE ( 'NONE', #1833, 5.000000000000000000 ) ;
#2316 = EDGE_CURVE ( 'NONE', #1588, #2799, #4170, .T. ) ;
#2317 = VECTOR ( 'NONE', #2186, 1000.000000000000000 ) ;
#2318 = CARTESIAN_POINT ( 'NONE',  ( 3.900000000000000799, 3.061616997868383141E-16, -2.500000000000000000 ) ) ;
#2319 = CARTESIAN_POINT ( 'NONE',  ( 0.5000000000000000000, 0.2499999999999982792, 1.911797424705720339 ) ) ;
#2320 = DIRECTION ( 'NONE',  ( 1.000000000000000000, 0.000000000000000000, 0.000000000000000000 ) ) ;
#2321 = AXIS2_PLACEMENT_3D ( 'NONE', #4119, #2350, #4083 ) ;
#2322 = CARTESIAN_POINT ( 'NONE',  ( 77.00000000000001421, 0.000000000000000000, -9.500000000000000000 ) ) ;
#2323 = CIRCLE ( 'NONE', #12, 5.000000000000000000 ) ;
#2324 = VERTEX_POINT ( 'NONE', #5529 ) ;
#2325 = CARTESIAN_POINT ( 'NONE',  ( 0.000000000000000000, 0.000000000000000000, 0.000000000000000000 ) ) ;
#2326 = DIRECTION ( 'NONE',  ( -1.000000000000000000, 0.000000000000000000, 0.000000000000000000 ) ) ;
#2327 = VECTOR ( 'NONE', #2847, 1000.000000000000000 ) ;
#2328 = VECTOR ( 'NONE', #4238, 1000.000000000000000 ) ;
#2329 = ORIENTED_EDGE ( 'NONE', *, *, #3538, .F. ) ;
#2330 = DIRECTION ( 'NONE',  ( 1.000000000000000000, -0.000000000000000000, -0.000000000000000000 ) ) ;
#2331 = AXIS2_PLACEMENT_3D ( 'NONE', #1110, #1958, #3391 ) ;
#2332 = AXIS2_PLACEMENT_3D ( 'NONE', #3388, #3029, #1987 ) ;
#2333 =( REPRESENTATION_RELATIONSHIP ('NONE','NONE', #5609, #2622 ) REPRESENTATION_RELATIONSHIP_WITH_TRANSFORMATION ( #942 )SHAPE_REPRESENTATION_RELATIONSHIP( ) );
#2334 = ORIENTED_EDGE ( 'NONE', *, *, #4810, .F. ) ;
#2335 = VECTOR ( 'NONE', #5787, 1000.000000000000227 ) ;
#2336 = CARTESIAN_POINT ( 'NONE',  ( 150.0000000000000284, 15.00000000000000000, 49.99999999999998579 ) ) ;
#2337 = AXIS2_PLACEMENT_3D ( 'NONE', #3473, #559, #5656 ) ;
#2338 = CARTESIAN_POINT ( 'NONE',  ( 75.00000000000001421, 0.000000000000000000, 0.000000000000000000 ) ) ;
#2339 = CONTEXT_DEPENDENT_SHAPE_REPRESENTATION ( #980, #3296 ) ;
#2340 = FILL_AREA_STYLE_COLOUR ( '', #2707 ) ;
#2341 = VERTEX_POINT ( 'NONE', #4141 ) ;
#2342 = MECHANICAL_DESIGN_GEOMETRIC_PRESENTATION_REPRESENTATION (  '', ( #5551 ), #2054 ) ;
#2343 = MECHANICAL_DESIGN_GEOMETRIC_PRESENTATION_REPRESENTATION (  '', ( #4482 ), #1179 ) ;
#2344 = ADVANCED_FACE ( 'NONE', ( #1371, #1122, #2920, #230 ), #707, .T. ) ;
#2345 = VERTEX_POINT ( 'NONE', #5703 ) ;
#2346 = EDGE_CURVE ( 'NONE', #52, #3182, #3347, .T. ) ;
#2347 = CIRCLE ( 'NONE', #2256, 7.500000000000000000 ) ;
#2348 = ADVANCED_FACE ( 'NONE', ( #2980, #4806 ), #3011, .F. ) ;
#2349 = EDGE_LOOP ( 'NONE', ( #3466, #5025, #4899, #1192 ) ) ;
#2350 = DIRECTION ( 'NONE',  ( -1.000000000000000000, -0.000000000000000000, -0.000000000000000000 ) ) ;
#2351 = ADVANCED_FACE ( 'NONE', ( #583 ), #5770, .T. ) ;
#2352 = CARTESIAN_POINT ( 'NONE',  ( 162.4999999999999716, 6.999999999999985789, 75.00000000000000000 ) ) ;
#2353 = LINE ( 'NONE', #3721, #2913 ) ;
#2354 = PLANE ( 'NONE',  #3313 ) ;
#2355 = STYLED_ITEM ( 'NONE', ( #2206 ), #4058 ) ;
#2356 = PLANE ( 'NONE',  #4666 ) ;
#2357 = ORIENTED_EDGE ( 'NONE', *, *, #1790, .F. ) ;
#2358 = CARTESIAN_POINT ( 'NONE',  ( 0.000000000000000000, 0.000000000000000000, 0.000000000000000000 ) ) ;
#2359 = AXIS2_PLACEMENT_3D ( 'NONE', #3783, #3845, #5130 ) ;
#2360 = DIRECTION ( 'NONE',  ( -0.000000000000000000, 1.000000000000000000, 1.224646799147353207E-16 ) ) ;
#2361 = ORIENTED_EDGE ( 'NONE', *, *, #910, .F. ) ;
#2362 = VECTOR ( 'NONE', #4861, 1000.000000000000000 ) ;
#2363 = CARTESIAN_POINT ( 'NONE',  ( 0.3609765494018736809, 0.2499999999999982792, 1.888098105530059190 ) ) ;
#2364 = EDGE_CURVE ( 'NONE', #782, #4209, #1440, .T. ) ;
#2365 = ORIENTED_EDGE ( 'NONE', *, *, #4397, .T. ) ;
#2366 = DIRECTION ( 'NONE',  ( 0.000000000000000000, 0.000000000000000000, -1.000000000000000000 ) ) ;
#2367 = ORIENTED_EDGE ( 'NONE', *, *, #390, .T. ) ;
#2368 = DIRECTION ( 'NONE',  ( 0.000000000000000000, 0.000000000000000000, -1.000000000000000000 ) ) ;
#2369 = DIRECTION ( 'NONE',  ( 0.000000000000000000, 0.000000000000000000, 1.000000000000000000 ) ) ;
#2370 = PRODUCT_DEFINITION_SHAPE ( 'NONE', 'NONE',  #5974 ) ;
#2371 =( NAMED_UNIT ( * ) PLANE_ANGLE_UNIT ( ) SI_UNIT ( $, .RADIAN. ) );
#2372 = LINE ( 'NONE', #3680, #503 ) ;
#2373 = ORIENTED_EDGE ( 'NONE', *, *, #1765, .F. ) ;
#2374 = EDGE_LOOP ( 'NONE', ( #2262, #5170, #4713, #2334 ) ) ;
#2375 = DIRECTION ( 'NONE',  ( -0.8949343913984706411, -1.557891129246106096E-15, 0.4461977533473793223 ) ) ;
#2376 = ADVANCED_FACE ( 'NONE', ( #2432 ), #4868, .T. ) ;
#2377 = ORIENTED_EDGE ( 'NONE', *, *, #3059, .F. ) ;
#2378 = CIRCLE ( 'NONE', #4716, 0.8509999999999999787 ) ;
#2379 = CARTESIAN_POINT ( 'NONE',  ( 137.4999999999999716, -6.999999999999985789, -65.00000000000000000 ) ) ;
#2380 = DIRECTION ( 'NONE',  ( 0.000000000000000000, 0.000000000000000000, -1.000000000000000000 ) ) ;
#2381 = DIRECTION ( 'NONE',  ( -1.000000000000000000, 0.000000000000000000, 0.000000000000000000 ) ) ;
#2382 = AXIS2_PLACEMENT_3D ( 'NONE', #149, #1986, #931 ) ;
#2383 = ORIENTED_EDGE ( 'NONE', *, *, #5393, .F. ) ;
#2384 = EDGE_CURVE ( 'NONE', #3113, #5408, #1031, .T. ) ;
#2385 = AXIS2_PLACEMENT_3D ( 'NONE', #1908, #1488, #5258 ) ;
#2386 = FACE_OUTER_BOUND ( 'NONE', #5197, .T. ) ;
#2387 = CIRCLE ( 'NONE', #1226, 0.5999999999999999778 ) ;
#2388 = CARTESIAN_POINT ( 'NONE',  ( 25.00000000000000711, -6.999999999999989342, -75.00000000000000000 ) ) ;
#2389 = DIRECTION ( 'NONE',  ( 0.000000000000000000, 0.000000000000000000, 1.000000000000000000 ) ) ;
#2390 = VERTEX_POINT ( 'NONE', #2032 ) ;
#2391 = ORIENTED_EDGE ( 'NONE', *, *, #3208, .F. ) ;
#2392 =( NAMED_UNIT ( * ) PLANE_ANGLE_UNIT ( ) SI_UNIT ( $, .RADIAN. ) );
#2393 = DIRECTION ( 'NONE',  ( 0.000000000000000000, 0.000000000000000000, 1.000000000000000000 ) ) ;
#2394 = EDGE_CURVE ( 'NONE', #666, #60, #5522, .T. ) ;
#2395 = VERTEX_POINT ( 'NONE', #191 ) ;
#2396 = DIRECTION ( 'NONE',  ( 0.000000000000000000, 0.000000000000000000, -1.000000000000000000 ) ) ;
#2397 = FACE_OUTER_BOUND ( 'NONE', #713, .T. ) ;
#2398 = CONTEXT_DEPENDENT_SHAPE_REPRESENTATION ( #4827, #2856 ) ;
#2399 = CARTESIAN_POINT ( 'NONE',  ( 37.50000000000000711, 6.288372600415927295E-15, -55.00000000000000000 ) ) ;
#2400 = DIRECTION ( 'NONE',  ( 0.4999999999999993894, 0.000000000000000000, -0.8660254037844389297 ) ) ;
#2401 = ORIENTED_EDGE ( 'NONE', *, *, #3250, .T. ) ;
#2402 = ORIENTED_EDGE ( 'NONE', *, *, #4399, .F. ) ;
#2403 = CARTESIAN_POINT ( 'NONE',  ( 2.740000000000000213, -0.5150000000000034550, 0.9838866223909985553 ) ) ;
#2404 = EDGE_LOOP ( 'NONE', ( #4237, #322, #5705, #2478 ) ) ;
#2405 = DIRECTION ( 'NONE',  ( 0.5000000000000003331, 0.000000000000000000, 0.8660254037844383745 ) ) ;
#2406 = CARTESIAN_POINT ( 'NONE',  ( 37.50000000000000711, 6.288372600415927295E-15, 75.00000000000000000 ) ) ;
#2407 = DIRECTION ( 'NONE',  ( 1.000000000000000000, 0.000000000000000000, -0.000000000000000000 ) ) ;
#2408 = ORIENTED_EDGE ( 'NONE', *, *, #4800, .F. ) ;
#2409 = VECTOR ( 'NONE', #2584, 1000.000000000000000 ) ;
#2410 = CARTESIAN_POINT ( 'NONE',  ( 0.000000000000000000, 0.000000000000000000, 0.000000000000000000 ) ) ;
#2411 = CARTESIAN_POINT ( 'NONE',  ( 67.00000000000001421, 0.000000000000000000, 0.000000000000000000 ) ) ;
#2412 =( REPRESENTATION_RELATIONSHIP ('NONE','NONE', #5609, #5016 ) REPRESENTATION_RELATIONSHIP_WITH_TRANSFORMATION ( #2886 )SHAPE_REPRESENTATION_RELATIONSHIP( ) );
#2413 = PRODUCT_DEFINITION ( 'UNKNOWN', '', #615, #1608 ) ;
#2414 = AXIS2_PLACEMENT_3D ( 'NONE', #2069, #5674, #4321 ) ;
#2415 = CARTESIAN_POINT ( 'NONE',  ( 60.00000000000001421, -1.645402210687070900E-15, 65.00000000000000000 ) ) ;
#2416 = CIRCLE ( 'NONE', #4163, 1.000000000000000000 ) ;
#2417 = CARTESIAN_POINT ( 'NONE',  ( 0.06760930072668894231, 0.9010842325122760954, 0.5149999999999993472 ) ) ;
#2418 = EDGE_CURVE ( 'NONE', #467, #5410, #3465, .T. ) ;
#2419 = ORIENTED_EDGE ( 'NONE', *, *, #4247, .T. ) ;
#2420 = ADVANCED_FACE ( 'NONE', ( #670 ), #5260, .T. ) ;
#2422 = EDGE_LOOP ( 'NONE', ( #307, #3684, #3948, #4372, #5003, #2849, #2923, #2505 ) ) ;
#2421 = PRODUCT_DEFINITION_SHAPE ( 'NONE', 'NONE',  #5984 ) ;
#2423 = AXIS2_PLACEMENT_3D ( 'NONE', #4705, #1988, #2874 ) ;
#2424 = DIRECTION ( 'NONE',  ( 0.000000000000000000, 0.000000000000000000, 1.000000000000000000 ) ) ;
#2425 = EDGE_CURVE ( 'NONE', #500, #698, #2610, .T. ) ;
#2426 = PRESENTATION_LAYER_ASSIGNMENT (  '', '', ( #5058 ) ) ;
#2427 = AXIS2_PLACEMENT_3D ( 'NONE', #3896, #4358, #2101 ) ;
#2428 = EDGE_LOOP ( 'NONE', ( #444, #4136 ) ) ;
#2429 = CYLINDRICAL_SURFACE ( 'NONE', #4096, 1.099999999999998535 ) ;
#2430 = DIRECTION ( 'NONE',  ( 0.000000000000000000, 0.000000000000000000, 1.000000000000000000 ) ) ;
#2431 = VECTOR ( 'NONE', #5812, 1000.000000000000000 ) ;
#2432 = FACE_OUTER_BOUND ( 'NONE', #1602, .T. ) ;
#2433 = PRESENTATION_STYLE_ASSIGNMENT (( #3525 ) ) ;
#2434 = ORIENTED_EDGE ( 'NONE', *, *, #2346, .F. ) ;
#2435 = EDGE_CURVE ( 'NONE', #5618, #3394, #3004, .T. ) ;
#2436 = VERTEX_POINT ( 'NONE', #3439 ) ;
#2437 = AXIS2_PLACEMENT_3D ( 'NONE', #5011, #5511, #2718 ) ;
#2438 = AXIS2_PLACEMENT_3D ( 'NONE', #584, #5675, #1007 ) ;
#2439 = CARTESIAN_POINT ( 'NONE',  ( 8.000000000000000000, -0.5149999999999999023, -1.857513327677604022E-15 ) ) ;
#2440 = VERTEX_POINT ( 'NONE', #2887 ) ;
#2441 = PLANE ( 'NONE',  #1267 ) ;
#2442 = CARTESIAN_POINT ( 'NONE',  ( 162.5000000000000000, 6.123233995736766282E-16, 5.000000000000000000 ) ) ;
#2443 = CARTESIAN_POINT ( 'NONE',  ( 0.000000000000000000, -15.00000000000000000, 0.000000000000000000 ) ) ;
#2444 = ORIENTED_EDGE ( 'NONE', *, *, #2872, .T. ) ;
#2445 = APPLICATION_PROTOCOL_DEFINITION ( 'draft international standard', 'automotive_design', 1998, #3579 ) ;
#2446 = DIRECTION ( 'NONE',  ( 0.000000000000000000, 0.000000000000000000, -1.000000000000000000 ) ) ;
#2447 = PRESENTATION_LAYER_ASSIGNMENT (  '', '', ( #2355 ) ) ;
#2448 = CARTESIAN_POINT ( 'NONE',  ( 0.5000000000000000000, 0.000000000000000000, 0.000000000000000000 ) ) ;
#2449 = DIRECTION ( 'NONE',  ( 0.000000000000000000, 0.000000000000000000, 1.000000000000000000 ) ) ;
#2450 = CARTESIAN_POINT ( 'NONE',  ( 150.0000000000000284, 15.00000000000000000, 49.99999999999998579 ) ) ;
#2451 = ORIENTED_EDGE ( 'NONE', *, *, #2162, .F. ) ;
#2452 = EDGE_LOOP ( 'NONE', ( #5202, #4313, #1786, #5741, #3673 ) ) ;
#2453 = VECTOR ( 'NONE', #4032, 1000.000000000000000 ) ;
#2454 = DIRECTION ( 'NONE',  ( -1.000000000000000000, 0.000000000000000000, 0.000000000000000000 ) ) ;
#2455 = UNCERTAINTY_MEASURE_WITH_UNIT (LENGTH_MEASURE( 1.000000000000000082E-05 ), #2489, 'distance_accuracy_value', 'NONE');
#2456 = EDGE_CURVE ( 'NONE', #51, #4013, #959, .T. ) ;
#2457 = ORIENTED_EDGE ( 'NONE', *, *, #4055, .T. ) ;
#2458 = EDGE_CURVE ( 'NONE', #1041, #695, #2952, .T. ) ;
#2459 = CARTESIAN_POINT ( 'NONE',  ( 24.99999999999998224, 6.999999999999985789, 65.00000000000000000 ) ) ;
#2460 = EDGE_CURVE ( 'NONE', #1098, #140, #1353, .T. ) ;
#2461 = PLANE ( 'NONE',  #3456 ) ;
#2462 = CARTESIAN_POINT ( 'NONE',  ( 75.00000000000001421, 0.000000000000000000, -9.500000000000000000 ) ) ;
#2463 = ORIENTED_EDGE ( 'NONE', *, *, #4160, .F. ) ;
#2464 = ORIENTED_EDGE ( 'NONE', *, *, #5604, .F. ) ;
#2465 = EDGE_CURVE ( 'NONE', #360, #554, #5645, .T. ) ;
#2466 = PLANE ( 'NONE',  #1437 ) ;
#2467 = CARTESIAN_POINT ( 'NONE',  ( 25.00000000000000711, -6.999999999999988454, 65.00000000000000000 ) ) ;
#2468 = LINE ( 'NONE', #3416, #4285 ) ;
#2469 = DIRECTION ( 'NONE',  ( 0.000000000000000000, 0.000000000000000000, 1.000000000000000000 ) ) ;
#2470 = EDGE_LOOP ( 'NONE', ( #5525, #410 ) ) ;
#2471 = CARTESIAN_POINT ( 'NONE',  ( 195.0000000000000284, 0.000000000000000000, 0.000000000000000000 ) ) ;
#2472 = CARTESIAN_POINT ( 'NONE',  ( 24.99999999999998224, -7.000000000000006217, 65.00000000000000000 ) ) ;
#2473 = DIRECTION ( 'NONE',  ( -0.000000000000000000, 0.000000000000000000, 1.000000000000000000 ) ) ;
#2474 = CARTESIAN_POINT ( 'NONE',  ( -45.00000000000002842, 0.000000000000000000, -44.99999999999998579 ) ) ;
#2475 = DIRECTION ( 'NONE',  ( -1.000000000000000000, -0.000000000000000000, -0.000000000000000000 ) ) ;
#2476 = DIRECTION ( 'NONE',  ( 0.4461977533473793778, 0.8949343913984707521, -1.884057886186824742E-16 ) ) ;
#2477 = EDGE_LOOP ( 'NONE', ( #1906, #877 ) ) ;
#2478 = ORIENTED_EDGE ( 'NONE', *, *, #4898, .T. ) ;
#2479 = CARTESIAN_POINT ( 'NONE',  ( 162.4999999999999716, -7.000000000000013323, 65.00000000000000000 ) ) ;
#2480 = VECTOR ( 'NONE', #1091, 1000.000000000000000 ) ;
#2481 = EDGE_LOOP ( 'NONE', ( #379, #2127 ) ) ;
#2482 = AXIS2_PLACEMENT_3D ( 'NONE', #1107, #5754, #4337 ) ;
#2483 = EDGE_CURVE ( 'NONE', #3408, #1524, #2323, .T. ) ;
#2484 = CARTESIAN_POINT ( 'NONE',  ( -35.00000000000000711, 40.00000000000000000, -45.00000000000000000 ) ) ;
#2485 = DIRECTION ( 'NONE',  ( 1.000000000000000000, 0.000000000000000000, 0.000000000000000000 ) ) ;
#2486 = ORIENTED_EDGE ( 'NONE', *, *, #2522, .T. ) ;
#2487 = EDGE_LOOP ( 'NONE', ( #5907, #3232, #1128, #3539 ) ) ;
#2488 = EDGE_CURVE ( 'NONE', #542, #1461, #3977, .T. ) ;
#2489 =( LENGTH_UNIT ( ) NAMED_UNIT ( * ) SI_UNIT ( .MILLI., .METRE. ) );
#2490 = DIRECTION ( 'NONE',  ( -0.000000000000000000, -0.000000000000000000, 1.000000000000000000 ) ) ;
#2491 = VERTEX_POINT ( 'NONE', #5406 ) ;
#2492 = CARTESIAN_POINT ( 'NONE',  ( 37.50000000000000711, 6.288372600415927295E-15, 71.29999999999999716 ) ) ;
#2493 = PLANE ( 'NONE',  #2337 ) ;
#2494 = FACE_OUTER_BOUND ( 'NONE', #2011, .T. ) ;
#2495 = VERTEX_POINT ( 'NONE', #1215 ) ;
#2496 = EDGE_CURVE ( 'NONE', #5415, #674, #5023, .T. ) ;
#2497 = LINE ( 'NONE', #2966, #1808 ) ;
#2498 = DIRECTION ( 'NONE',  ( -0.000000000000000000, -0.000000000000000000, -1.000000000000000000 ) ) ;
#2499 = DIRECTION ( 'NONE',  ( 0.000000000000000000, -0.000000000000000000, 1.000000000000000000 ) ) ;
#2500 = CARTESIAN_POINT ( 'NONE',  ( 24.99999999999998224, -7.000000000000006217, 75.00000000000000000 ) ) ;
#2501 = DIRECTION ( 'NONE',  ( 1.007709689656716815E-16, 1.000000000000000000, 3.606821995490527259E-15 ) ) ;
#2502 = CIRCLE ( 'NONE', #4261, 0.9999999999999991118 ) ;
#2503 = ORIENTED_EDGE ( 'NONE', *, *, #932, .F. ) ;
#2504 = EDGE_CURVE ( 'NONE', #2228, #5607, #4176, .T. ) ;
#2505 = ORIENTED_EDGE ( 'NONE', *, *, #1526, .F. ) ;
#2506 = SHAPE_REPRESENTATION_RELATIONSHIP ( 'NONE' , 'NONE' ,  #5882, #1882 ) ;
#2507 = CARTESIAN_POINT ( 'NONE',  ( 8.000000000000000000, -4.837354856632045452E-15, 0.000000000000000000 ) ) ;
#2508 = AXIS2_PLACEMENT_3D ( 'NONE', #4379, #312, #1121 ) ;
#2509 = EDGE_LOOP ( 'NONE', ( #4749, #2007, #2624 ) ) ;
#2510 = AXIS2_PLACEMENT_3D ( 'NONE', #5120, #2716, #3291 ) ;
#2511 = AXIS2_PLACEMENT_3D ( 'NONE', #4402, #5849, #4852 ) ;
#2512 = CARTESIAN_POINT ( 'NONE',  ( -36.33974596215562514, 45.00000000000000000, 44.99999999999999289 ) ) ;
#2513 = MECHANICAL_DESIGN_GEOMETRIC_PRESENTATION_REPRESENTATION (  '', ( #5058 ), #3689 ) ;
#2514 = AXIS2_PLACEMENT_3D ( 'NONE', #29, #4725, #1038 ) ;
#2515 = DIRECTION ( 'NONE',  ( 0.000000000000000000, 0.000000000000000000, 1.000000000000000000 ) ) ;
#2516 = ORIENTED_EDGE ( 'NONE', *, *, #4245, .T. ) ;
#2517 = ORIENTED_EDGE ( 'NONE', *, *, #1583, .T. ) ;
#2518 = CIRCLE ( 'NONE', #1849, 5.000000000000004441 ) ;
#2519 = VECTOR ( 'NONE', #1069, 1000.000000000000000 ) ;
#2520 = DIRECTION ( 'NONE',  ( 0.000000000000000000, -1.000000000000000000, -3.491481338843133355E-15 ) ) ;
#2521 = DIRECTION ( 'NONE',  ( -1.000000000000000000, 0.000000000000000000, -0.000000000000000000 ) ) ;
#2522 = EDGE_CURVE ( 'NONE', #5881, #3531, #1550, .T. ) ;
#2523 = VERTEX_POINT ( 'NONE', #3073 ) ;
#2524 = VECTOR ( 'NONE', #4486, 1000.000000000000341 ) ;
#2525 = CIRCLE ( 'NONE', #3228, 0.9999999999999991118 ) ;
#2526 = CARTESIAN_POINT ( 'NONE',  ( 55.00000000000000711, 0.000000000000000000, 0.000000000000000000 ) ) ;
#2527 = EDGE_CURVE ( 'NONE', #4082, #1856, #5798, .T. ) ;
#2528 = DIRECTION ( 'NONE',  ( 0.000000000000000000, 0.000000000000000000, -1.000000000000000000 ) ) ;
#2529 = EDGE_CURVE ( 'NONE', #823, #5679, #2715, .T. ) ;
#2530 =( REPRESENTATION_RELATIONSHIP ('NONE','NONE', #5609, #5882 ) REPRESENTATION_RELATIONSHIP_WITH_TRANSFORMATION ( #442 )SHAPE_REPRESENTATION_RELATIONSHIP( ) );
#2531 = CARTESIAN_POINT ( 'NONE',  ( 135.4999999999999716, 0.000000000000000000, -7.000000000000000000 ) ) ;
#2532 = ORIENTED_EDGE ( 'NONE', *, *, #826, .T. ) ;
#2533 = VECTOR ( 'NONE', #1233, 1000.000000000000000 ) ;
#2534 = PRODUCT_CONTEXT ( 'NONE', #2846, 'mechanical' ) ;
#2535 = EDGE_CURVE ( 'NONE', #1175, #4444, #4996, .T. ) ;
#2536 = VECTOR ( 'NONE', #3227, 1000.000000000000000 ) ;
#2537 = CARTESIAN_POINT ( 'NONE',  ( 0.3226060873438401089, 2.189154565102731098, -0.5150000000000000133 ) ) ;
#2538 = DIRECTION ( 'NONE',  ( 0.000000000000000000, 0.000000000000000000, -1.000000000000000000 ) ) ;
#2539 = DIRECTION ( 'NONE',  ( 0.000000000000000000, 0.000000000000000000, 1.000000000000000000 ) ) ;
#2540 = DIRECTION ( 'NONE',  ( -1.000000000000000000, 0.000000000000000000, 0.000000000000000000 ) ) ;
#2542 = AXIS2_PLACEMENT_3D ( 'NONE', #693, #5309, #1601 ) ;
#2541 = DIRECTION ( 'NONE',  ( 0.8949343913984143528, 0.4461977533474921764, 1.416481476476136321E-16 ) ) ;
#2543 = ORIENTED_EDGE ( 'NONE', *, *, #753, .T. ) ;
#2544 = B_SPLINE_CURVE_WITH_KNOTS ( 'NONE', 3,
 ( #1439, #1505, #1955, #3301 ),
 .UNSPECIFIED., .F., .F.,
 ( 4, 4 ),
 ( 0.004656695506220393486, 0.007337072593346776264 ),
 .UNSPECIFIED. ) ;
#2545 = ORIENTED_EDGE ( 'NONE', *, *, #2831, .F. ) ;
#2546 =( NAMED_UNIT ( * ) SI_UNIT ( $, .STERADIAN. ) SOLID_ANGLE_UNIT ( ) );
#2547 = FACE_BOUND ( 'NONE', #4417, .T. ) ;
#2548 = EDGE_CURVE ( 'NONE', #360, #5930, #5858, .T. ) ;
#2549 = ORIENTED_EDGE ( 'NONE', *, *, #4247, .F. ) ;
#2550 =( LENGTH_UNIT ( ) NAMED_UNIT ( * ) SI_UNIT ( .MILLI., .METRE. ) );
#2551 = LINE ( 'NONE', #4413, #3965 ) ;
#2552 = DIRECTION ( 'NONE',  ( 0.000000000000000000, 0.000000000000000000, -1.000000000000000000 ) ) ;
#2553 = ORIENTED_EDGE ( 'NONE', *, *, #4220, .T. ) ;
#2554 = VECTOR ( 'NONE', #4314, 1000.000000000000000 ) ;
#2555 = VERTEX_POINT ( 'NONE', #760 ) ;
#2556 = DIRECTION ( 'NONE',  ( 0.000000000000000000, -3.606821995490527259E-15, 1.000000000000000000 ) ) ;
#2557 = LINE ( 'NONE', #260, #2123 ) ;
#2558 = CLOSED_SHELL ( 'NONE', ( #4050, #810, #2681, #5719, #4047, #1320, #5759, #2881, #334, #5678 ) ) ;
#2559 = ORIENTED_EDGE ( 'NONE', *, *, #2067, .T. ) ;
#2560 = DIRECTION ( 'NONE',  ( 1.000000000000000000, 0.000000000000000000, 0.000000000000000000 ) ) ;
#2561 = CARTESIAN_POINT ( 'NONE',  ( 1.794155980045909482, 0.000000000000000000, 0.000000000000000000 ) ) ;
#2562 = DIRECTION ( 'NONE',  ( 0.000000000000000000, 0.000000000000000000, -1.000000000000000000 ) ) ;
#2563 = VERTEX_POINT ( 'NONE', #2609 ) ;
#2564 = SHAPE_DEFINITION_REPRESENTATION ( #1500, #2622 ) ;
#2565 = CYLINDRICAL_SURFACE ( 'NONE', #5680, 1.000000000000000000 ) ;
#2566 = EDGE_CURVE ( 'NONE', #5507, #3782, #1730, .T. ) ;
#2567 = CARTESIAN_POINT ( 'NONE',  ( 8.000000000000000000, -4.837354856632045452E-15, -0.5150000000000000133 ) ) ;
#2568 = DIRECTION ( 'NONE',  ( -0.000000000000000000, -0.000000000000000000, 1.000000000000000000 ) ) ;
#2569 = CARTESIAN_POINT ( 'NONE',  ( 0.5477065543514070267, 0.000000000000000000, -1.934182851860892116 ) ) ;
#2570 = PRODUCT_DEFINITION ( 'UNKNOWN', '', #2164, #5792 ) ;
#2571 = PLANE ( 'NONE',  #3695 ) ;
#2572 = ORIENTED_EDGE ( 'NONE', *, *, #1156, .F. ) ;
#2573 = ORIENTED_EDGE ( 'NONE', *, *, #2088, .F. ) ;
#2574 =( NAMED_UNIT ( * ) SI_UNIT ( $, .STERADIAN. ) SOLID_ANGLE_UNIT ( ) );
#2575 = DIRECTION ( 'NONE',  ( -0.000000000000000000, -1.000000000000000000, -0.000000000000000000 ) ) ;
#2576 = EDGE_LOOP ( 'NONE', ( #4204, #1208, #5753, #2210 ) ) ;
#2577 =( NAMED_UNIT ( * ) PLANE_ANGLE_UNIT ( ) SI_UNIT ( $, .RADIAN. ) );
#2578 = EDGE_CURVE ( 'NONE', #1480, #635, #4505, .T. ) ;
#2579 = DIRECTION ( 'NONE',  ( 1.000000000000000000, -0.000000000000000000, -0.000000000000000000 ) ) ;
#2580 = AXIS2_PLACEMENT_3D ( 'NONE', #2786, #4641, #3477 ) ;
#2581 = DIRECTION ( 'NONE',  ( 0.000000000000000000, 1.000000000000000000, 0.000000000000000000 ) ) ;
#2582 = ORIENTED_EDGE ( 'NONE', *, *, #2167, .T. ) ;
#2583 = EDGE_LOOP ( 'NONE', ( #415, #1851 ) ) ;
#2584 = DIRECTION ( 'NONE',  ( -0.8571673013836870192, 1.049727191973306873E-16, 0.5150380737757234151 ) ) ;
#2585 = ORIENTED_EDGE ( 'NONE', *, *, #1610, .F. ) ;
#2586 = CARTESIAN_POINT ( 'NONE',  ( 9.299999999999998934, 1.000000000000000000, 0.000000000000000000 ) ) ;
#2587 = CARTESIAN_POINT ( 'NONE',  ( 62.50000000000001421, -1.951563910473909559E-15, -55.00000000000000000 ) ) ;
#2588 = EDGE_LOOP ( 'NONE', ( #5585, #1354, #4536, #4616 ) ) ;
#2589 = LINE ( 'NONE', #4452, #5827 ) ;
#2590 = ORIENTED_EDGE ( 'NONE', *, *, #3660, .T. ) ;
#2591 = ITEM_DEFINED_TRANSFORMATION ( 'NONE', 'NONE', #1392,  #5080 ) ;
#2592 = PLANE ( 'NONE',  #364 ) ;
#2593 = DIRECTION ( 'NONE',  ( -1.000000000000000000, -0.000000000000000000, -0.000000000000000000 ) ) ;
#2594 = PLANE ( 'NONE',  #4655 ) ;
#2595 = UNCERTAINTY_MEASURE_WITH_UNIT (LENGTH_MEASURE( 1.000000000000000082E-05 ), #3361, 'distance_accuracy_value', 'NONE');
#2596 = CARTESIAN_POINT ( 'NONE',  ( 77.00000000000001421, 0.000000000000000000, 8.400000000000000355 ) ) ;
#2597 = FACE_BOUND ( 'NONE', #1216, .T. ) ;
#2598 = VERTEX_POINT ( 'NONE', #2157 ) ;
#2599 = SURFACE_STYLE_FILL_AREA ( #4527 ) ;
#2600 = FACE_OUTER_BOUND ( 'NONE', #4017, .T. ) ;
#2601 = EDGE_LOOP ( 'NONE', ( #4126, #5782 ) ) ;
#2602 = EDGE_CURVE ( 'NONE', #5213, #1033, #2614, .T. ) ;
#2603 = SURFACE_SIDE_STYLE ('',( #5646 ) ) ;
#2604 = EDGE_CURVE ( 'NONE', #1794, #3819, #851, .T. ) ;
#2605 = SURFACE_STYLE_FILL_AREA ( #758 ) ;
#2606 = CIRCLE ( 'NONE', #2310, 4.999999999999990230 ) ;
#2607 = FACE_OUTER_BOUND ( 'NONE', #184, .T. ) ;
#2608 = ADVANCED_FACE ( 'NONE', ( #348, #3139 ), #4037, .T. ) ;
#2609 = CARTESIAN_POINT ( 'NONE',  ( 1.299999999999999156, 0.000000000000000000, -2.000000000000000000 ) ) ;
#2610 = CIRCLE ( 'NONE', #4169, 1.099999999999998535 ) ;
#2611 = ORIENTED_EDGE ( 'NONE', *, *, #5498, .T. ) ;
#2612 = ORIENTED_EDGE ( 'NONE', *, *, #224, .T. ) ;
#2613 = CARTESIAN_POINT ( 'NONE',  ( -45.00000000000001421, 40.00000000000000000, 45.00000000000000000 ) ) ;
#2614 = CIRCLE ( 'NONE', #1153, 12.00000000000000000 ) ;
#2615 = DIRECTION ( 'NONE',  ( 0.000000000000000000, -2.105246936865057050E-16, -1.000000000000000000 ) ) ;
#2616 = ORIENTED_EDGE ( 'NONE', *, *, #4653, .T. ) ;
#2617 = CARTESIAN_POINT ( 'NONE',  ( 135.4999999999999716, 8.572527594031473190E-16, 7.000000000000000000 ) ) ;
#2618 = EDGE_CURVE ( 'NONE', #1705, #2634, #4754, .T. ) ;
#2619 = CARTESIAN_POINT ( 'NONE',  ( 150.0000000000000284, 15.00000000000000000, 40.00000000000000711 ) ) ;
#2620 = ORIENTED_EDGE ( 'NONE', *, *, #3681, .F. ) ;
#2621 = CARTESIAN_POINT ( 'NONE',  ( 0.2309054577385447060, -0.2499999999999997780, -1.812959136724909159 ) ) ;
#2622 = SHAPE_REPRESENTATION ( 'lock', ( #5080 ), #332 ) ;
#2623 = AXIS2_PLACEMENT_3D ( 'NONE', #2838, #5566, #4668 ) ;
#2624 = ORIENTED_EDGE ( 'NONE', *, *, #1348, .T. ) ;
#2625 = APPLICATION_PROTOCOL_DEFINITION ( 'draft international standard', 'automotive_design', 1998, #555 ) ;
#2626 = CARTESIAN_POINT ( 'NONE',  ( -40.66987298107780902, 45.00000000000000000, 52.49999999999999289 ) ) ;
#2627 = AXIS2_PLACEMENT_3D ( 'NONE', #3595, #2104, #835 ) ;
#2628 = VECTOR ( 'NONE', #2656, 1000.000000000000000 ) ;
#2629 = CARTESIAN_POINT ( 'NONE',  ( -45.00000000000001421, 30.00000000000000355, 45.00000000000000000 ) ) ;
#2630 = DIRECTION ( 'NONE',  ( 0.000000000000000000, 0.000000000000000000, -1.000000000000000000 ) ) ;
#2631 = CARTESIAN_POINT ( 'NONE',  ( 43.00000000000000000, 6.288372600415927295E-15, 71.29999999999999716 ) ) ;
#2632 = DIRECTION ( 'NONE',  ( 0.000000000000000000, -1.000000000000000000, 0.000000000000000000 ) ) ;
#2633 = AXIS2_PLACEMENT_3D ( 'NONE', #5358, #4906, #352 ) ;
#2634 = VERTEX_POINT ( 'NONE', #4066 ) ;
#2635 = CIRCLE ( 'NONE', #4084, 5.000000000000004441 ) ;
#2636 = PRESENTATION_LAYER_ASSIGNMENT (  '', '', ( #4482 ) ) ;
#2637 = DIRECTION ( 'NONE',  ( 1.000000000000000000, -0.000000000000000000, -0.000000000000000000 ) ) ;
#2638 = AXIS2_PLACEMENT_3D ( 'NONE', #850, #2701, #2211 ) ;
#2639=STYLED_ITEM('',(#5999),#272);
#2640 = AXIS2_PLACEMENT_3D ( 'NONE', #1665, #3961, #1782 ) ;
#2641 = AXIS2_PLACEMENT_3D ( 'NONE', #4733, #5664, #5632 ) ;
#2642 = VERTEX_POINT ( 'NONE', #2125 ) ;
#2643 = DIRECTION ( 'NONE',  ( -1.000000000000000000, 0.000000000000000000, 0.000000000000000000 ) ) ;
#2644 = CARTESIAN_POINT ( 'NONE',  ( 67.00000000000001421, 0.000000000000000000, 0.000000000000000000 ) ) ;
#2645 = EDGE_CURVE ( 'NONE', #3979, #1825, #4415, .T. ) ;
#2646 = CARTESIAN_POINT ( 'NONE',  ( 37.50000000000000711, 6.288372600415927295E-15, -55.00000000000000000 ) ) ;
#2647 =( GEOMETRIC_REPRESENTATION_CONTEXT ( 3 ) GLOBAL_UNCERTAINTY_ASSIGNED_CONTEXT ( ( #2026 ) ) GLOBAL_UNIT_ASSIGNED_CONTEXT ( ( #2116, #5374, #4344 ) ) REPRESENTATION_CONTEXT ( 'NONE', 'WORKASPACE' ) );
#2649 = ORIENTED_EDGE ( 'NONE', *, *, #3835, .T. ) ;
#2648 = EDGE_CURVE ( 'NONE', #2799, #3083, #1604, .T. ) ;
#2650 = VERTEX_POINT ( 'NONE', #3166 ) ;
#2651 = CARTESIAN_POINT ( 'NONE',  ( -45.00000000000001421, 45.00000000000000000, 39.99999999999999289 ) ) ;
#2652 = CARTESIAN_POINT ( 'NONE',  ( 67.00000000000001421, 0.000000000000000000, 0.000000000000000000 ) ) ;
#2653 = APPLICATION_CONTEXT ( 'automotive_design' ) ;
#2654 = SURFACE_STYLE_USAGE ( .BOTH. , #3562 ) ;
#2655 = ORIENTED_EDGE ( 'NONE', *, *, #5921, .T. ) ;
#2656 = DIRECTION ( 'NONE',  ( 0.9961946980917455452, 0.000000000000000000, -0.08715574274765848506 ) ) ;
#2657 = DIRECTION ( 'NONE',  ( -0.000000000000000000, -0.000000000000000000, -1.000000000000000000 ) ) ;
#2658 = VERTEX_POINT ( 'NONE', #3645 ) ;
#2659 = DIRECTION ( 'NONE',  ( -1.000000000000000000, -0.000000000000000000, -0.000000000000000000 ) ) ;
#2660 = ORIENTED_EDGE ( 'NONE', *, *, #5731, .F. ) ;
#2661 = ADVANCED_FACE ( 'NONE', ( #5210 ), #2904, .F. ) ;
#2662 = EDGE_CURVE ( 'NONE', #4209, #2523, #1957, .T. ) ;
#2663 = DIRECTION ( 'NONE',  ( 0.000000000000000000, 0.000000000000000000, 1.000000000000000000 ) ) ;
#2664 = DIRECTION ( 'NONE',  ( -1.000000000000000000, 4.770489558936220126E-17, 0.000000000000000000 ) ) ;
#2665 = DIRECTION ( 'NONE',  ( -0.000000000000000000, -1.000000000000000000, -0.000000000000000000 ) ) ;
#2666 = DIRECTION ( 'NONE',  ( 0.000000000000000000, 0.000000000000000000, 1.000000000000000000 ) ) ;
#2667 = ORIENTED_EDGE ( 'NONE', *, *, #876, .F. ) ;
#2668 = FACE_OUTER_BOUND ( 'NONE', #3798, .T. ) ;
#2669 = VERTEX_POINT ( 'NONE', #3811 ) ;
#2670 = DIRECTION ( 'NONE',  ( 1.000000000000000000, -0.000000000000000000, -0.000000000000000000 ) ) ;
#2671 = DIRECTION ( 'NONE',  ( 0.000000000000000000, 0.000000000000000000, 1.000000000000000000 ) ) ;
#2672 = CARTESIAN_POINT ( 'NONE',  ( 137.4999999999999716, 0.000000000000000000, 0.000000000000000000 ) ) ;
#2673 = ORIENTED_EDGE ( 'NONE', *, *, #5542, .T. ) ;
#2674 = ORIENTED_EDGE ( 'NONE', *, *, #2618, .F. ) ;
#2675 = CARTESIAN_POINT ( 'NONE',  ( 20.85786437626904899, 0.000000000000000000, 0.000000000000000000 ) ) ;
#2676 = AXIS2_PLACEMENT_3D ( 'NONE', #2013, #5366, #4398 ) ;
#2677 = SURFACE_STYLE_FILL_AREA ( #4110 ) ;
#2678 = VERTEX_POINT ( 'NONE', #4103 ) ;
#2679 = CARTESIAN_POINT ( 'NONE',  ( 25.00000000000000711, -6.999999999999988454, -65.00000000000000000 ) ) ;
#2680 = CARTESIAN_POINT ( 'NONE',  ( -45.00000000000001421, 15.00000000000000000, 45.00000000000000000 ) ) ;
#2681 = ADVANCED_FACE ( 'NONE', ( #5662 ), #5954, .T. ) ;
#2682 = ORIENTED_EDGE ( 'NONE', *, *, #2764, .T. ) ;
#2683 = PLANE ( 'NONE',  #3226 ) ;
#2684 = EDGE_CURVE ( 'NONE', #2958, #2749, #3839, .T. ) ;
#2685 = VERTEX_POINT ( 'NONE', #437 ) ;
#2686 = DIRECTION ( 'NONE',  ( 0.000000000000000000, 0.000000000000000000, 1.000000000000000000 ) ) ;
#2687 = EDGE_CURVE ( 'NONE', #1289, #3398, #4758, .T. ) ;
#2688 = DIRECTION ( 'NONE',  ( 0.000000000000000000, 0.000000000000000000, 1.000000000000000000 ) ) ;
#2689 = PLANE ( 'NONE',  #5819 ) ;
#2690 = FACE_OUTER_BOUND ( 'NONE', #3594, .T. ) ;
#2691 = CIRCLE ( 'NONE', #1330, 0.4499999999999985678 ) ;
#2692 = PLANE ( 'NONE',  #3320 ) ;
#2693 = EDGE_CURVE ( 'NONE', #5479, #1856, #1792, .T. ) ;
#2694 = ORIENTED_EDGE ( 'NONE', *, *, #315, .F. ) ;
#2695 =( LENGTH_UNIT ( ) NAMED_UNIT ( * ) SI_UNIT ( .MILLI., .METRE. ) );
#2696 = DIRECTION ( 'NONE',  ( -0.000000000000000000, -0.000000000000000000, 1.000000000000000000 ) ) ;
#2697 = ORIENTED_EDGE ( 'NONE', *, *, #3252, .T. ) ;
#2698 = PLANE ( 'NONE',  #5162 ) ;
#2699 = EDGE_CURVE ( 'NONE', #4855, #5607, #1044, .T. ) ;
#2700 = VECTOR ( 'NONE', #5392, 1000.000000000000000 ) ;
#2701 = DIRECTION ( 'NONE',  ( -1.000000000000000000, -0.000000000000000000, -0.000000000000000000 ) ) ;
#2702 = CARTESIAN_POINT ( 'NONE',  ( 59.85000000000001563, -1.627032508699861061E-15, 75.00000000000000000 ) ) ;
#2703 = ORIENTED_EDGE ( 'NONE', *, *, #2602, .T. ) ;
#2704 = VECTOR ( 'NONE', #588, 1000.000000000000000 ) ;
#2705 = ORIENTED_EDGE ( 'NONE', *, *, #2725, .T. ) ;
#2706 = DIRECTION ( 'NONE',  ( 1.000000000000000000, -0.000000000000000000, -0.000000000000000000 ) ) ;
#2707 = COLOUR_RGB ( '',0.8941176470588234615, 0.8941176470588234615, 0.8941176470588234615 ) ;
#2708 = ORIENTED_EDGE ( 'NONE', *, *, #2120, .F. ) ;
#2709 = DIRECTION ( 'NONE',  ( 1.000000000000000000, -0.000000000000000000, -0.000000000000000000 ) ) ;
#2710 = LINE ( 'NONE', #4609, #5539 ) ;
#2711 = ORIENTED_EDGE ( 'NONE', *, *, #1790, .T. ) ;
#2712 = CARTESIAN_POINT ( 'NONE',  ( 25.00000000000000711, 7.000000000000009770, 75.00000000000000000 ) ) ;
#2713 = AXIS2_PLACEMENT_3D ( 'NONE', #3740, #513, #5589 ) ;
#2714 = ORIENTED_EDGE ( 'NONE', *, *, #5738, .F. ) ;
#2715 = CIRCLE ( 'NONE', #4957, 5.499999999999998224 ) ;
#2716 = DIRECTION ( 'NONE',  ( 0.000000000000000000, -1.000000000000000000, -3.491481338843133355E-15 ) ) ;
#2717 = ADVANCED_FACE ( 'NONE', ( #3390, #4134 ), #5597, .F. ) ;
#2718 = DIRECTION ( 'NONE',  ( 0.000000000000000000, 0.000000000000000000, 1.000000000000000000 ) ) ;
#2719 = EDGE_CURVE ( 'NONE', #5410, #1820, #5160, .T. ) ;
#2720 = AXIS2_PLACEMENT_3D ( 'NONE', #4391, #714, #1653 ) ;
#2721 = DIRECTION ( 'NONE',  ( 1.000000000000000000, 0.000000000000000000, 0.000000000000000000 ) ) ;
#2722 = PLANE ( 'NONE',  #2248 ) ;
#2723 = DIRECTION ( 'NONE',  ( 0.000000000000000000, -1.000000000000000000, -5.421010862427519705E-17 ) ) ;
#2724 = ORIENTED_EDGE ( 'NONE', *, *, #4765, .F. ) ;
#2725 = EDGE_CURVE ( 'NONE', #3970, #939, #4851, .T. ) ;
#2726 = AXIS2_PLACEMENT_3D ( 'NONE', #302, #341, #2204 ) ;
#2727 = SHAPE_DEFINITION_REPRESENTATION ( #4552, #5016 ) ;
#2728 = TOROIDAL_SURFACE ( 'NONE', #113, 2.700000000000000178, 0.2000000000000000111 ) ;
#2729 = CARTESIAN_POINT ( 'NONE',  ( 0.06760930072668894231, 0.9010842325122760954, 0.5149999999999993472 ) ) ;
#2730 = ORIENTED_EDGE ( 'NONE', *, *, #141, .T. ) ;
#2731 = VECTOR ( 'NONE', #3055, 1000.000000000000000 ) ;
#2733 = AXIS2_PLACEMENT_3D ( 'NONE', #446, #2261, #2773 ) ;
#2732 = FACE_BOUND ( 'NONE', #4315, .T. ) ;
#2734 = APPLICATION_CONTEXT ( 'automotive_design' ) ;
#2735 = CIRCLE ( 'NONE', #2437, 5.000000000000004441 ) ;
#2736 =( NAMED_UNIT ( * ) SI_UNIT ( $, .STERADIAN. ) SOLID_ANGLE_UNIT ( ) );
#2737 = DIRECTION ( 'NONE',  ( -1.000000000000000000, 0.000000000000000000, 0.000000000000000000 ) ) ;
#2738 = PRESENTATION_LAYER_ASSIGNMENT (  '', '', ( #2639 ) ) ;
#2739 = AXIS2_PLACEMENT_3D ( 'NONE', #5700, #488, #3371 ) ;
#2740 = AXIS2_PLACEMENT_3D ( 'NONE', #3813, #3276, #5128 ) ;
#2741 = EDGE_CURVE ( 'NONE', #3113, #4824, #3106, .T. ) ;
#2742 = CARTESIAN_POINT ( 'NONE',  ( 0.06760930072668813740, -0.5150000000000026779, 0.9010842325122891960 ) ) ;
#2743 = AXIS2_PLACEMENT_3D ( 'NONE', #1305, #3165, #1728 ) ;
#2744 = VERTEX_POINT ( 'NONE', #4309 ) ;
#2745 = ORIENTED_EDGE ( 'NONE', *, *, #2687, .T. ) ;
#2746 = FACE_OUTER_BOUND ( 'NONE', #3891, .T. ) ;
#2747 = COLOUR_RGB ( '',0.8941176470588234615, 0.8941176470588234615, 0.8941176470588234615 ) ;
#2748 = DIRECTION ( 'NONE',  ( 1.000000000000000000, 0.000000000000000000, 0.000000000000000000 ) ) ;
#2749 = VERTEX_POINT ( 'NONE', #151 ) ;
#2750 = DIRECTION ( 'NONE',  ( 0.000000000000000000, 0.000000000000000000, -1.000000000000000000 ) ) ;
#2751 = DIRECTION ( 'NONE',  ( 0.000000000000000000, 0.000000000000000000, 1.000000000000000000 ) ) ;
#2752 = ORIENTED_EDGE ( 'NONE', *, *, #4959, .F. ) ;
#2753 = CARTESIAN_POINT ( 'NONE',  ( -1.470152734901925752E-14, 0.2499999999999982792, -1.453737367178236983 ) ) ;
#2754 = ORIENTED_EDGE ( 'NONE', *, *, #2864, .T. ) ;
#2755 =( LENGTH_UNIT ( ) NAMED_UNIT ( * ) SI_UNIT ( .MILLI., .METRE. ) );
#2756 = FACE_OUTER_BOUND ( 'NONE', #2583, .T. ) ;
#2757 = CARTESIAN_POINT ( 'NONE',  ( 62.50000000000001421, -1.951563910473909559E-15, 55.00000000000000000 ) ) ;
#2758 = DIRECTION ( 'NONE',  ( 1.000000000000000000, -0.000000000000000000, -0.000000000000000000 ) ) ;
#2759 = CARTESIAN_POINT ( 'NONE',  ( -45.00000000000001421, 30.00000000000000355, 50.00000000000000000 ) ) ;
#2760 = ORIENTED_EDGE ( 'NONE', *, *, #4370, .F. ) ;
#2761 = DIRECTION ( 'NONE',  ( 0.000000000000000000, 1.000000000000000000, 0.000000000000000000 ) ) ;
#2762 = CLOSED_SHELL ( 'NONE', ( #4840, #3428, #5467, #3190, #470, #2351, #3280, #2792, #4172, #1381 ) ) ;
#2763 = CARTESIAN_POINT ( 'NONE',  ( 75.00000000000001421, -15.00000000000000355, 75.00000000000000000 ) ) ;
#2764 = EDGE_CURVE ( 'NONE', #3819, #4354, #5186, .T. ) ;
#2765 = PRESENTATION_STYLE_ASSIGNMENT (( #1329 ) ) ;
#2766 = DIRECTION ( 'NONE',  ( 0.000000000000000000, -1.000000000000000000, 0.000000000000000000 ) ) ;
#2767 = EDGE_CURVE ( 'NONE', #1033, #5213, #2227, .T. ) ;
#2768 = ORIENTED_EDGE ( 'NONE', *, *, #4653, .F. ) ;
#2769 = CYLINDRICAL_SURFACE ( 'NONE', #2153, 5.000000000000000000 ) ;
#2770 = ITEM_DEFINED_TRANSFORMATION ( 'NONE', 'NONE', #3904,  #5080 ) ;
#2771 = CARTESIAN_POINT ( 'NONE',  ( -40.66987298107780902, 40.00000000000000000, 52.49999999999999289 ) ) ;
#2772 = VERTEX_POINT ( 'NONE', #1332 ) ;
#2773 = DIRECTION ( 'NONE',  ( 0.000000000000000000, -3.552713678800500929E-15, -1.000000000000000000 ) ) ;
#2774 = ORIENTED_EDGE ( 'NONE', *, *, #4664, .T. ) ;
#2775 = VERTEX_POINT ( 'NONE', #4248 ) ;
#2776 = VECTOR ( 'NONE', #63, 1000.000000000000000 ) ;
#2777 = DIRECTION ( 'NONE',  ( 0.000000000000000000, -1.000000000000000000, 0.000000000000000000 ) ) ;
#2778 = PLANE ( 'NONE',  #4554 ) ;
#2779 = CARTESIAN_POINT ( 'NONE',  ( 2.740000000000000213, 0.5150000000000035660, -0.9838866223905657904 ) ) ;
#2780 = CIRCLE ( 'NONE', #3556, 5.000000000000004441 ) ;
#2781 = CARTESIAN_POINT ( 'NONE',  ( 8.000000000000000000, -4.837354856632045452E-15, 0.000000000000000000 ) ) ;
#2782 = DIRECTION ( 'NONE',  ( 1.000000000000000000, 0.000000000000000000, 0.000000000000000000 ) ) ;
#2783 = EDGE_LOOP ( 'NONE', ( #1609, #3056 ) ) ;
#2784 = DIRECTION ( 'NONE',  ( 0.000000000000000000, 0.000000000000000000, -1.000000000000000000 ) ) ;
#2785 = SHAPE_REPRESENTATION ( 'guide track', ( #5080 ), #3707 ) ;
#2786 = CARTESIAN_POINT ( 'NONE',  ( 150.0000000000000284, 15.00000000000000000, 45.00000000000000000 ) ) ;
#2787 = CARTESIAN_POINT ( 'NONE',  ( -74.99999999999998579, -15.00000000000000000, 75.00000000000000000 ) ) ;
#2788 = VERTEX_POINT ( 'NONE', #4732 ) ;
#2789 =( LENGTH_UNIT ( ) NAMED_UNIT ( * ) SI_UNIT ( .MILLI., .METRE. ) );
#2790 = CARTESIAN_POINT ( 'NONE',  ( 2.740000000000000213, 0.6774776749089226335, -0.5150000000000000133 ) ) ;
#2791 = EDGE_CURVE ( 'NONE', #4755, #2495, #4562, .T. ) ;
#2792 = ADVANCED_FACE ( 'NONE', ( #408, #2250 ), #5053, .T. ) ;
#2793 = EDGE_CURVE ( 'NONE', #3745, #3162, #3870, .T. ) ;
#2794 = ORIENTED_EDGE ( 'NONE', *, *, #141, .F. ) ;
#2795 = DIRECTION ( 'NONE',  ( 0.000000000000000000, 0.000000000000000000, -1.000000000000000000 ) ) ;
#2796 = EDGE_CURVE ( 'NONE', #171, #1741, #1109, .T. ) ;
#2797 = DIRECTION ( 'NONE',  ( 0.000000000000000000, 1.000000000000000000, 0.000000000000000000 ) ) ;
#2798 = DIRECTION ( 'NONE',  ( 0.000000000000000000, 0.000000000000000000, 1.000000000000000000 ) ) ;
#2799 = VERTEX_POINT ( 'NONE', #5721 ) ;
#2800 = CIRCLE ( 'NONE', #5416, 10.00000000000000178 ) ;
#2801 = LINE ( 'NONE', #4144, #3506 ) ;
#2802 = EDGE_LOOP ( 'NONE', ( #3718, #1138 ) ) ;
#2803 = ORIENTED_EDGE ( 'NONE', *, *, #5010, .T. ) ;
#2804 = CARTESIAN_POINT ( 'NONE',  ( 137.4999999999999716, -15.00000000000000000, 75.00000000000001421 ) ) ;
#2805 = AXIS2_PLACEMENT_3D ( 'NONE', #3677, #17, #972 ) ;
#2806 = ADVANCED_FACE ( 'NONE', ( #2110 ), #4340, .F. ) ;
#2807 = LINE ( 'NONE', #5971, #3286 ) ;
#2808 = DIRECTION ( 'NONE',  ( 1.000000000000000000, -0.000000000000000000, -0.000000000000000000 ) ) ;
#2809 = FACE_BOUND ( 'NONE', #3116, .T. ) ;
#2810 = LINE ( 'NONE', #31, #1165 ) ;
#2811 = VECTOR ( 'NONE', #4443, 1000.000000000000000 ) ;
#2812 = ORIENTED_EDGE ( 'NONE', *, *, #301, .T. ) ;
#2813 = DIRECTION ( 'NONE',  ( 1.000000000000000000, 0.000000000000000000, 0.000000000000000000 ) ) ;
#2814 = DIRECTION ( 'NONE',  ( -1.000000000000000000, -0.000000000000000000, -0.000000000000000000 ) ) ;
#2815 = AXIS2_PLACEMENT_3D ( 'NONE', #2959, #262, #2987 ) ;
#2816 = CARTESIAN_POINT ( 'NONE',  ( 137.4999999999999716, 15.00000000000000000, -75.00000000000000000 ) ) ;
#2817 = AXIS2_PLACEMENT_3D ( 'NONE', #3424, #1666, #5282 ) ;
#2818 = VECTOR ( 'NONE', #3451, 1000.000000000000000 ) ;
#2819 = EDGE_LOOP ( 'NONE', ( #3590, #5383, #1647, #2655 ) ) ;
#2820 =( LENGTH_UNIT ( ) NAMED_UNIT ( * ) SI_UNIT ( .MILLI., .METRE. ) );
#2821 = CYLINDRICAL_SURFACE ( 'NONE', #3128, 2.500000000000002220 ) ;
#2822 = VECTOR ( 'NONE', #2659, 1000.000000000000000 ) ;
#2823 = CIRCLE ( 'NONE', #883, 1.928074011315806136 ) ;
#2824 = ORIENTED_EDGE ( 'NONE', *, *, #5501, .F. ) ;
#2825 = AXIS2_PLACEMENT_3D ( 'NONE', #1469, #4151, #1867 ) ;
#2826 = DIRECTION ( 'NONE',  ( 0.000000000000000000, 0.000000000000000000, 1.000000000000000000 ) ) ;
#2827 = AXIS2_PLACEMENT_3D ( 'NONE', #4019, #4422, #289 ) ;
#2828 = LINE ( 'NONE', #759, #3935 ) ;
#2829 = ADVANCED_FACE ( 'NONE', ( #3030 ), #1930, .F. ) ;
#2830 = DIRECTION ( 'NONE',  ( 1.000000000000000000, 0.000000000000000000, 0.000000000000000000 ) ) ;
#2831 = EDGE_CURVE ( 'NONE', #5067, #2028, #5054, .T. ) ;
#2832 = AXIS2_PLACEMENT_3D ( 'NONE', #4501, #345, #2277 ) ;
#2833 = PLANE ( 'NONE',  #1760 ) ;
#2834 = ORIENTED_EDGE ( 'NONE', *, *, #3250, .F. ) ;
#2835 = ORIENTED_EDGE ( 'NONE', *, *, #3907, .T. ) ;
#2836 = PLANE ( 'NONE',  #399 ) ;
#2837 = CARTESIAN_POINT ( 'NONE',  ( 1.084202172485504434E-16, 0.000000000000000000, 0.000000000000000000 ) ) ;
#2838 = CARTESIAN_POINT ( 'NONE',  ( 150.0000000000000284, 15.00000000000000000, 45.00000000000000000 ) ) ;
#2839 = LINE ( 'NONE', #1409, #222 ) ;
#2840 = ADVANCED_FACE ( 'NONE', ( #577 ), #2429, .F. ) ;
#2841 = PLANE ( 'NONE',  #4098 ) ;
#2842 = ORIENTED_EDGE ( 'NONE', *, *, #2976, .F. ) ;
#2843 = ADVANCED_FACE ( 'NONE', ( #4428 ), #2594, .T. ) ;
#2844 = DIRECTION ( 'NONE',  ( 0.000000000000000000, 0.000000000000000000, 1.000000000000000000 ) ) ;
#2845 = CARTESIAN_POINT ( 'NONE',  ( -45.00000000000001421, 40.00000000000000000, -45.00000000000000000 ) ) ;
#2846 = APPLICATION_CONTEXT ( 'automotive_design' ) ;
#2847 = DIRECTION ( 'NONE',  ( -0.000000000000000000, -0.000000000000000000, -1.000000000000000000 ) ) ;
#2848 = CARTESIAN_POINT ( 'NONE',  ( 162.5000000000000000, 7.000000000000013323, 75.00000000000001421 ) ) ;
#2849 = ORIENTED_EDGE ( 'NONE', *, *, #4434, .F. ) ;
#2850 = EDGE_LOOP ( 'NONE', ( #728, #2133, #1397 ) ) ;
#2851 = DIRECTION ( 'NONE',  ( -1.000000000000000000, 0.000000000000000000, 0.000000000000000000 ) ) ;
#2852 = VERTEX_POINT ( 'NONE', #5814 ) ;
#2853 = DIRECTION ( 'NONE',  ( -0.000000000000000000, -1.000000000000000000, -0.000000000000000000 ) ) ;
#2854 = CARTESIAN_POINT ( 'NONE',  ( 62.50000000000001421, -1.951563910473909559E-15, 55.00000000000000000 ) ) ;
#2855 = CONTEXT_DEPENDENT_SHAPE_REPRESENTATION ( #3353, #5141 ) ;
#2856 = PRODUCT_DEFINITION_SHAPE ( 'NONE', 'NONE',  #5992 ) ;
#2857 = FACE_OUTER_BOUND ( 'NONE', #2509, .T. ) ;
#2858 = FILL_AREA_STYLE_COLOUR ( '', #1074 ) ;
#2859 = ORIENTED_EDGE ( 'NONE', *, *, #1151, .F. ) ;
#2860 = ORIENTED_EDGE ( 'NONE', *, *, #1568, .T. ) ;
#2861 = FACE_OUTER_BOUND ( 'NONE', #1240, .T. ) ;
#2862 = PRODUCT_RELATED_PRODUCT_CATEGORY ( 'part', '', ( #682 ) ) ;
#2863 = CARTESIAN_POINT ( 'NONE',  ( -25.39999999999996305, 0.000000000000000000, 2.500000000000000000 ) ) ;
#2864 = EDGE_CURVE ( 'NONE', #1472, #3630, #2029, .T. ) ;
#2865 = ORIENTED_EDGE ( 'NONE', *, *, #4106, .T. ) ;
#2866 = CARTESIAN_POINT ( 'NONE',  ( 67.00000000000000000, 0.000000000000000000, -10.49999999999999822 ) ) ;
#2867 = ADVANCED_FACE ( 'NONE', ( #630 ), #180, .T. ) ;
#2868 = DIRECTION ( 'NONE',  ( 1.000000000000000000, 0.000000000000000000, 0.000000000000000000 ) ) ;
#2869 = CARTESIAN_POINT ( 'NONE',  ( 62.50000000000001421, -1.951563910473909559E-15, 75.00000000000000000 ) ) ;
#2870 = AXIS2_PLACEMENT_3D ( 'NONE', #5127, #958, #2446 ) ;
#2871 = ORIENTED_EDGE ( 'NONE', *, *, #5050, .F. ) ;
#2872 = EDGE_CURVE ( 'NONE', #2634, #1705, #4366, .T. ) ;
#2873 = FACE_BOUND ( 'NONE', #1811, .T. ) ;
#2874 = DIRECTION ( 'NONE',  ( 0.000000000000000000, 0.000000000000000000, -1.000000000000000000 ) ) ;
#2875 = CARTESIAN_POINT ( 'NONE',  ( 162.4999999999999716, -7.000000000000013323, 75.00000000000000000 ) ) ;
#2876 = ORIENTED_EDGE ( 'NONE', *, *, #2687, .F. ) ;
#2877 = ORIENTED_EDGE ( 'NONE', *, *, #2978, .F. ) ;
#2878 = SHAPE_REPRESENTATION_RELATIONSHIP ( 'NONE' , 'NONE' ,  #2622, #3558 ) ;
#2879 = DIRECTION ( 'NONE',  ( 0.000000000000000000, 1.000000000000000000, 0.000000000000000000 ) ) ;
#2880 = UNCERTAINTY_MEASURE_WITH_UNIT (LENGTH_MEASURE( 1.000000000000000082E-05 ), #3851, 'distance_accuracy_value', 'NONE');
#2881 = ADVANCED_FACE ( 'NONE', ( #5338, #2968 ), #2015, .F. ) ;
#2882 = VECTOR ( 'NONE', #2579, 1000.000000000000000 ) ;
#2883 = VERTEX_POINT ( 'NONE', #1631 ) ;
#2884 = DIRECTION ( 'NONE',  ( 0.000000000000000000, -1.000000000000000000, 0.000000000000000000 ) ) ;
#2885 = CARTESIAN_POINT ( 'NONE',  ( -45.00000000000001421, 40.00000000000000000, 45.00000000000000000 ) ) ;
#2886 = ITEM_DEFINED_TRANSFORMATION ( 'NONE', 'NONE', #338,  #5080 ) ;
#2887 = CARTESIAN_POINT ( 'NONE',  ( 75.00000000000001421, 15.00000000000000000, -75.00000000000000000 ) ) ;
#2888 = SURFACE_SIDE_STYLE ('',( #104 ) ) ;
#2889 = ORIENTED_EDGE ( 'NONE', *, *, #537, .T. ) ;
#2890 = ORIENTED_EDGE ( 'NONE', *, *, #1823, .T. ) ;
#2891 = DIRECTION ( 'NONE',  ( -0.000000000000000000, -0.000000000000000000, -1.000000000000000000 ) ) ;
#2892 = DIRECTION ( 'NONE',  ( -1.000000000000000000, 0.000000000000000000, 0.000000000000000000 ) ) ;
#2893 = ORIENTED_EDGE ( 'NONE', *, *, #5879, .T. ) ;
#2894 = DIRECTION ( 'NONE',  ( 0.000000000000000000, 0.000000000000000000, 1.000000000000000000 ) ) ;
#2895 = CARTESIAN_POINT ( 'NONE',  ( 24.99999999999998224, 6.999999999999985789, 75.00000000000000000 ) ) ;
#2896 = CARTESIAN_POINT ( 'NONE',  ( -45.00000000000001421, 40.00000000000000000, -45.00000000000000000 ) ) ;
#2897 = ORIENTED_EDGE ( 'NONE', *, *, #301, .F. ) ;
#2898 = COLOUR_RGB ( '',0.8941176470588234615, 0.8941176470588234615, 0.8941176470588234615 ) ;
#2899 = EDGE_CURVE ( 'NONE', #4444, #3189, #582, .T. ) ;
#2900 = APPLICATION_PROTOCOL_DEFINITION ( 'draft international standard', 'automotive_design', 1998, #2846 ) ;
#2901 = DIRECTION ( 'NONE',  ( 0.000000000000000000, 0.000000000000000000, -1.000000000000000000 ) ) ;
#2902 = EDGE_CURVE ( 'NONE', #1820, #3160, #5307, .T. ) ;
#2903 = CONICAL_SURFACE ( 'NONE', #774, 2.500000000000002220, 1.029744260000002631 ) ;
#2904 = CYLINDRICAL_SURFACE ( 'NONE', #1057, 5.000000000000004441 ) ;
#2905 = CARTESIAN_POINT ( 'NONE',  ( 75.00000000000001421, 0.000000000000000000, -10.49999999999999822 ) ) ;
#2906 = EDGE_CURVE ( 'NONE', #2003, #1041, #2141, .T. ) ;
#2907 = DIRECTION ( 'NONE',  ( 0.000000000000000000, 0.000000000000000000, -1.000000000000000000 ) ) ;
#2908 = ORIENTED_EDGE ( 'NONE', *, *, #3785, .T. ) ;
#2909 = ORIENTED_EDGE ( 'NONE', *, *, #2120, .T. ) ;
#2910 = PRESENTATION_STYLE_ASSIGNMENT (( #4767 ) ) ;
#2911 = LINE ( 'NONE', #5698, #4108 ) ;
#2912 = ORIENTED_EDGE ( 'NONE', *, *, #3322, .F. ) ;
#2913 = VECTOR ( 'NONE', #4750, 1000.000000000000000 ) ;
#2914 = ADVANCED_FACE ( 'NONE', ( #299 ), #5148, .F. ) ;
#2915 = DIRECTION ( 'NONE',  ( 0.000000000000000000, 0.000000000000000000, 1.000000000000000000 ) ) ;
#2916 = EDGE_CURVE ( 'NONE', #3278, #52, #2939, .T. ) ;
#2917 = DIRECTION ( 'NONE',  ( 0.000000000000000000, 0.000000000000000000, -1.000000000000000000 ) ) ;
#2918 = AXIS2_PLACEMENT_3D ( 'NONE', #3033, #2501, #5816 ) ;
#2919 = AXIS2_PLACEMENT_3D ( 'NONE', #2679, #380, #4018 ) ;
#2920 = FACE_OUTER_BOUND ( 'NONE', #5697, .T. ) ;
#2921 = LINE ( 'NONE', #1972, #1081 ) ;
#2922 = AXIS2_PLACEMENT_3D ( 'NONE', #3955, #4912, #1290 ) ;
#2923 = ORIENTED_EDGE ( 'NONE', *, *, #2741, .T. ) ;
#2924 = AXIS2_PLACEMENT_3D ( 'NONE', #1561, #1102, #5779 ) ;
#2925 = ORIENTED_EDGE ( 'NONE', *, *, #458, .F. ) ;
#2926 = DIRECTION ( 'NONE',  ( 1.000000000000000000, -0.000000000000000000, -0.000000000000000000 ) ) ;
#2927 = VECTOR ( 'NONE', #1169, 1000.000000000000000 ) ;
#2928 = AXIS2_PLACEMENT_3D ( 'NONE', #5616, #3041, #4718 ) ;
#2929 = DIRECTION ( 'NONE',  ( -0.000000000000000000, -0.000000000000000000, -1.000000000000000000 ) ) ;
#2930 = EDGE_LOOP ( 'NONE', ( #1934, #1333, #807, #3815 ) ) ;
#2931 = DIRECTION ( 'NONE',  ( 0.000000000000000000, 0.000000000000000000, 1.000000000000000000 ) ) ;
#2932 = DIRECTION ( 'NONE',  ( 0.000000000000000000, -5.421010862427519705E-17, 1.000000000000000000 ) ) ;
#2933 = CARTESIAN_POINT ( 'NONE',  ( 3.700000000000000178, 0.000000000000000000, 2.700000000000000178 ) ) ;
#2934 = ORIENTED_EDGE ( 'NONE', *, *, #3915, .T. ) ;
#2935 =( GEOMETRIC_REPRESENTATION_CONTEXT ( 3 ) GLOBAL_UNCERTAINTY_ASSIGNED_CONTEXT ( ( #5251 ) ) GLOBAL_UNIT_ASSIGNED_CONTEXT ( ( #4802, #227, #1182 ) ) REPRESENTATION_CONTEXT ( 'NONE', 'WORKASPACE' ) );
#2936 = APPLICATION_PROTOCOL_DEFINITION ( 'draft international standard', 'automotive_design', 1998, #5329 ) ;
#2937 = DIRECTION ( 'NONE',  ( 1.000000000000000000, -4.770489558936219510E-17, 0.000000000000000000 ) ) ;
#2938 = CARTESIAN_POINT ( 'NONE',  ( -35.00000000000000711, 40.00000000000000000, 45.00000000000000000 ) ) ;
#2939 = LINE ( 'NONE', #3871, #298 ) ;
#2940 = CARTESIAN_POINT ( 'NONE',  ( 2.740000000000000213, 0.9838866223910003317, 0.5149999999999999023 ) ) ;
#2941 = FACE_OUTER_BOUND ( 'NONE', #3622, .T. ) ;
#2942 = EDGE_LOOP ( 'NONE', ( #344, #2964, #1112, #2667 ) ) ;
#2943 = AXIS2_PLACEMENT_3D ( 'NONE', #2358, #2844, #4218 ) ;
#2944 = ORIENTED_EDGE ( 'NONE', *, *, #135, .T. ) ;
#2945 = AXIS2_PLACEMENT_3D ( 'NONE', #4949, #3938, #1638 ) ;
#2946 = CARTESIAN_POINT ( 'NONE',  ( -996.9834933385058093, 0.000000000000000000, 0.000000000000000000 ) ) ;
#2947 = UNCERTAINTY_MEASURE_WITH_UNIT (LENGTH_MEASURE( 1.000000000000000082E-05 ), #880, 'distance_accuracy_value', 'NONE');
#2948 = PRODUCT_RELATED_PRODUCT_CATEGORY ( 'part', '', ( #1399 ) ) ;
#2949 = VERTEX_POINT ( 'NONE', #1135 ) ;
#2950 = ADVANCED_FACE ( 'NONE', ( #2996 ), #3479, .F. ) ;
#2951 = LINE ( 'NONE', #3283, #3925 ) ;
#2952 = LINE ( 'NONE', #5292, #3969 ) ;
#2953 = EDGE_CURVE ( 'NONE', #1325, #5963, #1847, .T. ) ;
#2954 = VERTEX_POINT ( 'NONE', #813 ) ;
#2955 = ORIENTED_EDGE ( 'NONE', *, *, #531, .F. ) ;
#2956 = FILL_AREA_STYLE ('',( #1099 ) ) ;
#2957 = CARTESIAN_POINT ( 'NONE',  ( 162.5000000000000000, -15.00000000000000000, -75.00000000000000000 ) ) ;
#2958 = VERTEX_POINT ( 'NONE', #2202 ) ;
#2959 = CARTESIAN_POINT ( 'NONE',  ( 75.00000000000001421, 0.000000000000000000, -9.500000000000000000 ) ) ;
#2960 = ADVANCED_FACE ( 'NONE', ( #4150 ), #778, .F. ) ;
#2961 = FACE_OUTER_BOUND ( 'NONE', #5295, .T. ) ;
#2962 = APPLICATION_CONTEXT ( 'automotive_design' ) ;
#2963 = DIRECTION ( 'NONE',  ( -1.000000000000000000, 0.000000000000000000, 0.000000000000000000 ) ) ;
#2964 = ORIENTED_EDGE ( 'NONE', *, *, #5599, .T. ) ;
#2965 = DIRECTION ( 'NONE',  ( 6.123233995736766036E-17, 0.000000000000000000, -1.000000000000000000 ) ) ;
#2966 = CARTESIAN_POINT ( 'NONE',  ( 24.99999999999998224, 7.000000000000006217, -65.00000000000000000 ) ) ;
#2967 = CARTESIAN_POINT ( 'NONE',  ( 75.00000000000001421, 0.000000000000000000, 9.500000000000000000 ) ) ;
#2968 = FACE_OUTER_BOUND ( 'NONE', #1149, .T. ) ;
#2969 = CIRCLE ( 'NONE', #3359, 2.500000000000002220 ) ;
#2970 = CYLINDRICAL_SURFACE ( 'NONE', #5350, 4.999999999999990230 ) ;
#2971 = FACE_OUTER_BOUND ( 'NONE', #2422, .T. ) ;
#2972 = ORIENTED_EDGE ( 'NONE', *, *, #1696, .F. ) ;
#2973 = ORIENTED_EDGE ( 'NONE', *, *, #1819, .F. ) ;
#2974 = CARTESIAN_POINT ( 'NONE',  ( 77.00000000000001421, 1.347111479062087271E-16, -8.400000000000000355 ) ) ;
#2975 = ORIENTED_EDGE ( 'NONE', *, *, #396, .T. ) ;
#2976 = EDGE_CURVE ( 'NONE', #3503, #605, #1350, .T. ) ;
#2977 = DIRECTION ( 'NONE',  ( 0.000000000000000000, 1.000000000000000000, -0.000000000000000000 ) ) ;
#2978 = EDGE_CURVE ( 'NONE', #3182, #1037, #3121, .T. ) ;
#2979 = EDGE_CURVE ( 'NONE', #5526, #3444, #3186, .T. ) ;
#2980 = FACE_BOUND ( 'NONE', #448, .T. ) ;
#2982 = EDGE_LOOP ( 'NONE', ( #524, #589, #4632 ) ) ;
#2981 = ADVANCED_FACE ( 'NONE', ( #5936 ), #902, .T. ) ;
#2983 = ORIENTED_EDGE ( 'NONE', *, *, #5879, .F. ) ;
#2984 = DIRECTION ( 'NONE',  ( 1.000000000000000000, -3.469446951953614189E-16, 0.000000000000000000 ) ) ;
#2985 = CARTESIAN_POINT ( 'NONE',  ( 67.00000000000000000, 0.000000000000000000, -9.500000000000000000 ) ) ;
#2986 = ORIENTED_EDGE ( 'NONE', *, *, #5234, .T. ) ;
#2987 = DIRECTION ( 'NONE',  ( 0.000000000000000000, 0.000000000000000000, -1.000000000000000000 ) ) ;
#2988 = DIRECTION ( 'NONE',  ( 0.000000000000000000, 0.000000000000000000, 1.000000000000000000 ) ) ;
#2989 = CARTESIAN_POINT ( 'NONE',  ( 67.00000000000000000, 0.000000000000000000, 9.500000000000000000 ) ) ;
#2990 = ORIENTED_EDGE ( 'NONE', *, *, #1191, .T. ) ;
#2991 = DIRECTION ( 'NONE',  ( -1.000000000000000000, 0.000000000000000000, 0.000000000000000000 ) ) ;
#2992 = EDGE_CURVE ( 'NONE', #107, #94, #5898, .T. ) ;
#2993 = CARTESIAN_POINT ( 'NONE',  ( 1.849560077140141701, -0.5149999999999969047, -0.7556913915602436749 ) ) ;
#2994 = VECTOR ( 'NONE', #1362, 1000.000000000000000 ) ;
#2995 = CARTESIAN_POINT ( 'NONE',  ( -45.00000000000001421, 30.00000000000000355, -45.00000000000000000 ) ) ;
#2996 = FACE_OUTER_BOUND ( 'NONE', #929, .T. ) ;
#2997 = DIRECTION ( 'NONE',  ( 0.4461977533474923430, 3.124646727056501411E-15, -0.8949343913984144638 ) ) ;
#2998 = DIRECTION ( 'NONE',  ( -1.000000000000000000, 0.000000000000000000, 0.000000000000000000 ) ) ;
#2999 = VECTOR ( 'NONE', #985, 1000.000000000000000 ) ;
#3000 = ORIENTED_EDGE ( 'NONE', *, *, #5803, .T. ) ;
#3001 = CARTESIAN_POINT ( 'NONE',  ( 37.50000000000000711, 6.288372600415927295E-15, 75.00000000000000000 ) ) ;
#3002 = CARTESIAN_POINT ( 'NONE',  ( 2.740000000000000213, 0.6774776749089226335, -0.5150000000000000133 ) ) ;
#3003 = PRODUCT_DEFINITION_CONTEXT ( 'detailed design', #2962, 'design' ) ;
#3004 = CIRCLE ( 'NONE', #575, 7.000000000000000000 ) ;
#3005 = ORIENTED_EDGE ( 'NONE', *, *, #1717, .T. ) ;
#3006 = VECTOR ( 'NONE', #3197, 1000.000000000000000 ) ;
#3007 = LINE ( 'NONE', #3436, #226 ) ;
#3008 = DIRECTION ( 'NONE',  ( 0.000000000000000000, -1.000000000000000000, 0.000000000000000000 ) ) ;
#3009 = AXIS2_PLACEMENT_3D ( 'NONE', #3017, #5774, #2556 ) ;
#3010 = VECTOR ( 'NONE', #2269, 1000.000000000000000 ) ;
#3011 = PLANE ( 'NONE',  #2414 ) ;
#3012 = VERTEX_POINT ( 'NONE', #2176 ) ;
#3013 = EDGE_CURVE ( 'NONE', #2059, #3272, #965, .T. ) ;
#3014 = ORIENTED_EDGE ( 'NONE', *, *, #496, .T. ) ;
#3015 = VECTOR ( 'NONE', #3271, 1000.000000000000000 ) ;
#3016 = AXIS2_PLACEMENT_3D ( 'NONE', #1252, #832, #3206 ) ;
#3017 = CARTESIAN_POINT ( 'NONE',  ( 0.000000000000000000, -0.5149999999999909095, -2.349999999999999201 ) ) ;
#3018 = EDGE_CURVE ( 'NONE', #5679, #5534, #3602, .T. ) ;
#3019 = DIRECTION ( 'NONE',  ( 1.007709689656716938E-16, 1.000000000000000000, 3.606821995490528048E-15 ) ) ;
#3020 = VERTEX_POINT ( 'NONE', #4027 ) ;
#3021 = CARTESIAN_POINT ( 'NONE',  ( -45.00000000000001421, 30.00000000000000355, -39.99999999999999289 ) ) ;
#3022 = CARTESIAN_POINT ( 'NONE',  ( -45.00000000000001421, 40.00000000000000000, 45.00000000000000000 ) ) ;
#3023 = CARTESIAN_POINT ( 'NONE',  ( 7.345657149124338758, 1.312408941150044583, 0.000000000000000000 ) ) ;
#3024 = EDGE_LOOP ( 'NONE', ( #607, #3147, #1942, #2251 ) ) ;
#3025 = AXIS2_PLACEMENT_3D ( 'NONE', #73, #3757, #1967 ) ;
#3026 = PRODUCT_CONTEXT ( 'NONE', #2024, 'mechanical' ) ;
#3027 = CIRCLE ( 'NONE', #2150, 1.000000000000000000 ) ;
#3028 = CARTESIAN_POINT ( 'NONE',  ( 7.345657149124971141, -1.312408941149200814, 2.762944903268657774E-16 ) ) ;
#3029 = DIRECTION ( 'NONE',  ( -0.000000000000000000, 0.000000000000000000, 1.000000000000000000 ) ) ;
#3030 = FACE_OUTER_BOUND ( 'NONE', #2982, .T. ) ;
#3031 = DIRECTION ( 'NONE',  ( 1.000000000000000000, -0.000000000000000000, -0.000000000000000000 ) ) ;
#3032 = COLOUR_RGB ( '',0.8941176470588234615, 0.8941176470588234615, 0.8941176470588234615 ) ;
#3033 = CARTESIAN_POINT ( 'NONE',  ( 0.000000000000000000, -0.5149999999999909095, -2.349999999999999201 ) ) ;
#3034 = ADVANCED_FACE ( 'NONE', ( #1261 ), #4180, .F. ) ;
#3035 = EDGE_LOOP ( 'NONE', ( #2298, #2708, #4601, #4778 ) ) ;
#3036 = ORIENTED_EDGE ( 'NONE', *, *, #278, .T. ) ;
#3037 =( NAMED_UNIT ( * ) PLANE_ANGLE_UNIT ( ) SI_UNIT ( $, .RADIAN. ) );
#3038 = DIRECTION ( 'NONE',  ( -1.000000000000000000, -0.000000000000000000, -0.000000000000000000 ) ) ;
#3039 =( GEOMETRIC_REPRESENTATION_CONTEXT ( 3 ) GLOBAL_UNCERTAINTY_ASSIGNED_CONTEXT ( ( #1262 ) ) GLOBAL_UNIT_ASSIGNED_CONTEXT ( ( #1176, #3521, #2023 ) ) REPRESENTATION_CONTEXT ( 'NONE', 'WORKASPACE' ) );
#3040 = ORIENTED_EDGE ( 'NONE', *, *, #5426, .T. ) ;
#3041 = DIRECTION ( 'NONE',  ( 1.000000000000000000, 0.000000000000000000, 0.000000000000000000 ) ) ;
#3042 = CARTESIAN_POINT ( 'NONE',  ( 137.4999999999999716, -7.000000000000011546, 65.00000000000000000 ) ) ;
#3043 = CIRCLE ( 'NONE', #5277, 7.000000000000000000 ) ;
#3044 = CONTEXT_DEPENDENT_SHAPE_REPRESENTATION ( #3967, #5769 ) ;
#3045 =( REPRESENTATION_RELATIONSHIP ('NONE','NONE', #5609, #5269 ) REPRESENTATION_RELATIONSHIP_WITH_TRANSFORMATION ( #3117 )SHAPE_REPRESENTATION_RELATIONSHIP( ) );
#3046 = AXIS2_PLACEMENT_3D ( 'NONE', #4345, #3038, #186 ) ;
#3047 = DIRECTION ( 'NONE',  ( 0.000000000000000000, 0.000000000000000000, 1.000000000000000000 ) ) ;
#3048 = EDGE_LOOP ( 'NONE', ( #5809, #4137, #848, #610 ) ) ;
#3049 = ORIENTED_EDGE ( 'NONE', *, *, #1877, .T. ) ;
#3050 = DIRECTION ( 'NONE',  ( -1.000000000000000000, 0.000000000000000000, 0.000000000000000000 ) ) ;
#3051 = EDGE_LOOP ( 'NONE', ( #4913, #5188 ) ) ;
#3052 = DIRECTION ( 'NONE',  ( 0.000000000000000000, 0.000000000000000000, -1.000000000000000000 ) ) ;
#3053 = DIRECTION ( 'NONE',  ( -1.000000000000000000, 0.000000000000000000, 0.000000000000000000 ) ) ;
#3054 = EDGE_LOOP ( 'NONE', ( #1879, #382, #3067, #4938 ) ) ;
#3055 = DIRECTION ( 'NONE',  ( -0.000000000000000000, -0.000000000000000000, -1.000000000000000000 ) ) ;
#3056 = ORIENTED_EDGE ( 'NONE', *, *, #1791, .T. ) ;
#3057 = EDGE_CURVE ( 'NONE', #5651, #1813, #493, .T. ) ;
#3058 = DIRECTION ( 'NONE',  ( 0.000000000000000000, 0.000000000000000000, 1.000000000000000000 ) ) ;
#3059 = EDGE_CURVE ( 'NONE', #1478, #2304, #1150, .T. ) ;
#3060 = CARTESIAN_POINT ( 'NONE',  ( -40.66987298107781612, 45.00000000000000000, 37.50000000000000000 ) ) ;
#3061 = DIRECTION ( 'NONE',  ( 0.000000000000000000, 0.000000000000000000, -1.000000000000000000 ) ) ;
#3062 = DIRECTION ( 'NONE',  ( 0.000000000000000000, 0.000000000000000000, -1.000000000000000000 ) ) ;
#3063 = CARTESIAN_POINT ( 'NONE',  ( 37.50000000000000711, 6.288372600415927295E-15, 65.00000000000000000 ) ) ;
#3064 = EDGE_LOOP ( 'NONE', ( #3201, #4812, #4033, #2975 ) ) ;
#3065 = EDGE_CURVE ( 'NONE', #5793, #2003, #5041, .T. ) ;
#3066 = CARTESIAN_POINT ( 'NONE',  ( 25.00000000000000711, 7.000000000000009770, -75.00000000000000000 ) ) ;
#3067 = ORIENTED_EDGE ( 'NONE', *, *, #5438, .T. ) ;
#3068 = CARTESIAN_POINT ( 'NONE',  ( -45.00000000000001421, 40.00000000000000000, -39.99999999999999289 ) ) ;
#3069 = DIRECTION ( 'NONE',  ( 0.000000000000000000, 0.000000000000000000, 1.000000000000000000 ) ) ;
#3070 = DIRECTION ( 'NONE',  ( 0.000000000000000000, 0.000000000000000000, 1.000000000000000000 ) ) ;
#3071 = CONICAL_SURFACE ( 'NONE', #1221, 2.500000000000002220, 1.029744260000002631 ) ;
#3072 = ADVANCED_FACE ( 'NONE', ( #3086 ), #2689, .F. ) ;
#3073 = CARTESIAN_POINT ( 'NONE',  ( 60.00000000000001421, -1.645402210687070900E-15, 65.00000000000000000 ) ) ;
#3074 = ORIENTED_EDGE ( 'NONE', *, *, #5835, .F. ) ;
#3075 = ORIENTED_EDGE ( 'NONE', *, *, #1659, .T. ) ;
#3076 =( LENGTH_UNIT ( ) NAMED_UNIT ( * ) SI_UNIT ( .MILLI., .METRE. ) );
#3077 = LINE ( 'NONE', #4040, #3759 ) ;
#3078 = VERTEX_POINT ( 'NONE', #4548 ) ;
#3079 = LINE ( 'NONE', #1828, #1938 ) ;
#3080 = DIRECTION ( 'NONE',  ( -0.000000000000000000, -0.000000000000000000, 1.000000000000000000 ) ) ;
#3081 = ORIENTED_EDGE ( 'NONE', *, *, #1646, .F. ) ;
#3082 = CARTESIAN_POINT ( 'NONE',  ( 60.00000000000001421, -1.951563910473909559E-15, -55.00000000000000000 ) ) ;
#3083 = VERTEX_POINT ( 'NONE', #2231 ) ;
#3084 = CARTESIAN_POINT ( 'NONE',  ( 19.70000000000000284, 0.000000000000000000, 0.000000000000000000 ) ) ;
#3085 = DIRECTION ( 'NONE',  ( 0.000000000000000000, 0.000000000000000000, 1.000000000000000000 ) ) ;
#3086 = FACE_OUTER_BOUND ( 'NONE', #1627, .T. ) ;
#3087 = UNCERTAINTY_MEASURE_WITH_UNIT (LENGTH_MEASURE( 1.000000000000000082E-05 ), #430, 'distance_accuracy_value', 'NONE');
#3088 = CARTESIAN_POINT ( 'NONE',  ( -74.99999999999998579, -15.00000000000000000, -75.00000000000000000 ) ) ;
#3089 = DIRECTION ( 'NONE',  ( 0.000000000000000000, -2.664535259100375697E-15, -1.000000000000000000 ) ) ;
#3090 = EDGE_CURVE ( 'NONE', #4013, #3020, #1322, .T. ) ;
#3091 = ORIENTED_EDGE ( 'NONE', *, *, #1715, .T. ) ;
#3092 = ADVANCED_FACE ( 'NONE', ( #1890 ), #2441, .F. ) ;
#3093 = SURFACE_SIDE_STYLE ('',( #2599 ) ) ;
#3094 = EDGE_CURVE ( 'NONE', #5855, #3980, #784, .T. ) ;
#3095 = CARTESIAN_POINT ( 'NONE',  ( 1.424271237134740131, -4.556291390728484991, -5.579847667638274858E-16 ) ) ;
#3096 = ADVANCED_FACE ( 'NONE', ( #4301 ), #505, .T. ) ;
#3097 = CIRCLE ( 'NONE', #5324, 7.983406227920510467 ) ;
#3098 = ORIENTED_EDGE ( 'NONE', *, *, #1827, .T. ) ;
#3099 = CARTESIAN_POINT ( 'NONE',  ( -45.00000000000001421, 0.000000000000000000, 45.00000000000000000 ) ) ;
#3100 = VECTOR ( 'NONE', #3795, 1000.000000000000000 ) ;
#3101 = CARTESIAN_POINT ( 'NONE',  ( 62.50000000000001421, -1.951563910473909559E-15, 71.29999999999999716 ) ) ;
#3102 = CARTESIAN_POINT ( 'NONE',  ( 77.00000000000001421, 0.000000000000000000, 0.000000000000000000 ) ) ;
#3103 = ORIENTED_EDGE ( 'NONE', *, *, #5903, .T. ) ;
#3104 = EDGE_CURVE ( 'NONE', #5094, #1875, #4181, .T. ) ;
#3105 = ORIENTED_EDGE ( 'NONE', *, *, #3154, .T. ) ;
#3106 = CIRCLE ( 'NONE', #486, 1.928074011315806136 ) ;
#3107 = PRODUCT_DEFINITION_SHAPE ( 'NONE', 'NONE',  #3939 ) ;
#3108 = CARTESIAN_POINT ( 'NONE',  ( 0.06760930072668799862, 0.5149999999999969047, 0.9010842325122926377 ) ) ;
#3109 = VERTEX_POINT ( 'NONE', #1915 ) ;
#3110 = DIRECTION ( 'NONE',  ( -0.000000000000000000, -1.000000000000000000, -0.000000000000000000 ) ) ;
#3111 = DIRECTION ( 'NONE',  ( -1.000000000000000000, -0.000000000000000000, -0.000000000000000000 ) ) ;
#3112 = CIRCLE ( 'NONE', #492, 0.8509999999999999787 ) ;
#3113 = VERTEX_POINT ( 'NONE', #2319 ) ;
#3114 = CARTESIAN_POINT ( 'NONE',  ( 3.016506661494197328, 8.581769150706125103E-33, -7.007546303702493782E-17 ) ) ;
#3115 = CIRCLE ( 'NONE', #3302, 4.556291390728477886 ) ;
#3116 = EDGE_LOOP ( 'NONE', ( #3340, #4294 ) ) ;
#3117 = ITEM_DEFINED_TRANSFORMATION ( 'NONE', 'NONE', #1586,  #5080 ) ;
#3118 = VECTOR ( 'NONE', #5066, 1000.000000000000000 ) ;
#3119 = CONICAL_SURFACE ( 'NONE', #2238, 3077.683537175319998, 1.256637061435923686 ) ;
#3120 = CARTESIAN_POINT ( 'NONE',  ( 9.300000000000002487, 0.000000000000000000, 1.000000000000000000 ) ) ;
#3121 = LINE ( 'NONE', #3217, #3010 ) ;
#3122 = FACE_OUTER_BOUND ( 'NONE', #4657, .T. ) ;
#3123 = DIRECTION ( 'NONE',  ( 1.000000000000000000, -4.770489558936219510E-17, 0.000000000000000000 ) ) ;
#3124 = ORIENTED_EDGE ( 'NONE', *, *, #719, .F. ) ;
#3125 = AXIS2_PLACEMENT_3D ( 'NONE', #5938, #1205, #3603 ) ;
#3126 = AXIS2_PLACEMENT_3D ( 'NONE', #3022, #4880, #3508 ) ;
#3127 = CARTESIAN_POINT ( 'NONE',  ( 0.000000000000000000, 2.349999999999998312, -0.5150000000000000133 ) ) ;
#3128 = AXIS2_PLACEMENT_3D ( 'NONE', #572, #5192, #1002 ) ;
#3129 = VECTOR ( 'NONE', #3172, 1000.000000000000000 ) ;
#3130 = MECHANICAL_DESIGN_GEOMETRIC_PRESENTATION_REPRESENTATION (  '', ( #1863 ), #5837 ) ;
#3131 = VECTOR ( 'NONE', #2670, 1000.000000000000000 ) ;
#3132 = ORIENTED_EDGE ( 'NONE', *, *, #5321, .T. ) ;
#3133 = DIRECTION ( 'NONE',  ( 0.000000000000000000, 0.000000000000000000, -1.000000000000000000 ) ) ;
#3134 = VECTOR ( 'NONE', #2797, 1000.000000000000000 ) ;
#3135 = SURFACE_STYLE_FILL_AREA ( #1276 ) ;
#3136 = PRODUCT_RELATED_PRODUCT_CATEGORY ( 'part', '', ( #2234 ) ) ;
#3137 = CARTESIAN_POINT ( 'NONE',  ( 62.50000000000001421, -1.951563910473909559E-15, 75.00000000000000000 ) ) ;
#3138 = EDGE_CURVE ( 'NONE', #1403, #4174, #1674, .T. ) ;
#3139 = FACE_OUTER_BOUND ( 'NONE', #4475, .T. ) ;
#3140 = LINE ( 'NONE', #1369, #730 ) ;
#3141 = ORIENTED_EDGE ( 'NONE', *, *, #3461, .F. ) ;
#3142 = ORIENTED_EDGE ( 'NONE', *, *, #1360, .T. ) ;
#3143 = DIRECTION ( 'NONE',  ( -0.000000000000000000, -0.000000000000000000, 1.000000000000000000 ) ) ;
#3144 = VECTOR ( 'NONE', #1209, 1000.000000000000000 ) ;
#3145 = EDGE_CURVE ( 'NONE', #3289, #4082, #2353, .T. ) ;
#3146 = DIRECTION ( 'NONE',  ( 0.000000000000000000, 0.000000000000000000, 1.000000000000000000 ) ) ;
#3147 = ORIENTED_EDGE ( 'NONE', *, *, #2058, .T. ) ;
#3148 = CARTESIAN_POINT ( 'NONE',  ( 150.0000000000000284, 0.000000000000000000, 49.99999999999998579 ) ) ;
#3149 = FACE_OUTER_BOUND ( 'NONE', #2942, .T. ) ;
#3150 = ORIENTED_EDGE ( 'NONE', *, *, #3094, .T. ) ;
#3151 = CARTESIAN_POINT ( 'NONE',  ( -45.00000000000001421, 45.00000000000000000, 45.00000000000000000 ) ) ;
#3152 = EDGE_LOOP ( 'NONE', ( #4869, #1869 ) ) ;
#3153 = LINE ( 'NONE', #5472, #3134 ) ;
#3154 = EDGE_CURVE ( 'NONE', #5304, #3852, #1554, .T. ) ;
#3155 = CARTESIAN_POINT ( 'NONE',  ( 75.00000000000001421, 0.000000000000000000, 8.400000000000000355 ) ) ;
#3156 = AXIS2_PLACEMENT_3D ( 'NONE', #4253, #95, #1578 ) ;
#3157 = CARTESIAN_POINT ( 'NONE',  ( 0.05007909176323187272, -0.2500000000000000000, 1.595164775286565861 ) ) ;
#3158 = DIRECTION ( 'NONE',  ( 0.000000000000000000, 0.000000000000000000, 1.000000000000000000 ) ) ;
#3159 = DIRECTION ( 'NONE',  ( 1.000000000000000000, 0.000000000000000000, 0.000000000000000000 ) ) ;
#3160 = VERTEX_POINT ( 'NONE', #2379 ) ;
#3161 = PLANE ( 'NONE',  #4328 ) ;
#3162 = VERTEX_POINT ( 'NONE', #5623 ) ;
#3163 = FACE_BOUND ( 'NONE', #5469, .T. ) ;
#3164 =( REPRESENTATION_RELATIONSHIP ('NONE','NONE', #5609, #2622 ) REPRESENTATION_RELATIONSHIP_WITH_TRANSFORMATION ( #463 )SHAPE_REPRESENTATION_RELATIONSHIP( ) );
#3165 = DIRECTION ( 'NONE',  ( 1.000000000000000000, -0.000000000000000000, -0.000000000000000000 ) ) ;
#3166 = CARTESIAN_POINT ( 'NONE',  ( 75.00000000000001421, 0.000000000000000000, -10.49999999999999822 ) ) ;
#3167 = CIRCLE ( 'NONE', #2580, 4.999999999999990230 ) ;
#3168 = ORIENTED_EDGE ( 'NONE', *, *, #2864, .F. ) ;
#3169 = EDGE_CURVE ( 'NONE', #2395, #2685, #1949, .T. ) ;
#3170 = ORIENTED_EDGE ( 'NONE', *, *, #1897, .F. ) ;
#3171 = AXIS2_PLACEMENT_3D ( 'NONE', #5672, #3372, #5138 ) ;
#3172 = DIRECTION ( 'NONE',  ( 0.000000000000000000, -1.734723475976808080E-16, -1.000000000000000000 ) ) ;
#3173 = EDGE_CURVE ( 'NONE', #3020, #2642, #1161, .T. ) ;
#3174 = CIRCLE ( 'NONE', #663, 5.000000000000000000 ) ;
#3175 = LINE ( 'NONE', #1312, #3865 ) ;
#3176 = EDGE_LOOP ( 'NONE', ( #2553, #4671 ) ) ;
#3177 = PRODUCT_RELATED_PRODUCT_CATEGORY ( 'part', '', ( #1635 ) ) ;
#3178 = FACE_OUTER_BOUND ( 'NONE', #1430, .T. ) ;
#3179 = CARTESIAN_POINT ( 'NONE',  ( 2.740000000000000213, 0.000000000000000000, 0.000000000000000000 ) ) ;
#3180 = EDGE_LOOP ( 'NONE', ( #4513, #3847 ) ) ;
#3181 = DIRECTION ( 'NONE',  ( 0.000000000000000000, 0.000000000000000000, -1.000000000000000000 ) ) ;
#3182 = VERTEX_POINT ( 'NONE', #3269 ) ;
#3183 = DIRECTION ( 'NONE',  ( 0.000000000000000000, -0.000000000000000000, -1.000000000000000000 ) ) ;
#3184 = SHAPE_REPRESENTATION ( 'plunger rod', ( #5080 ), #4591 ) ;
#3185 = LINE ( 'NONE', #5484, #5487 ) ;
#3186 = LINE ( 'NONE', #4493, #4662 ) ;
#3187 = CARTESIAN_POINT ( 'NONE',  ( 135.4999999999999716, 0.000000000000000000, -7.000000000000000000 ) ) ;
#3188 = DIRECTION ( 'NONE',  ( 0.000000000000000000, -1.000000000000000000, 0.000000000000000000 ) ) ;
#3189 = VERTEX_POINT ( 'NONE', #56 ) ;
#3190 = ADVANCED_FACE ( 'NONE', ( #114 ), #1384, .T. ) ;
#3191 = SHAPE_REPRESENTATION_RELATIONSHIP ( 'NONE' , 'NONE' ,  #4225, #3198 ) ;
#3192 = DIRECTION ( 'NONE',  ( 0.000000000000000000, -3.612465276695121047E-15, 1.000000000000000000 ) ) ;
#3193 = ORIENTED_EDGE ( 'NONE', *, *, #824, .T. ) ;
#3194 = FACE_OUTER_BOUND ( 'NONE', #535, .T. ) ;
#3195 =( NAMED_UNIT ( * ) SI_UNIT ( $, .STERADIAN. ) SOLID_ANGLE_UNIT ( ) );
#3196 = LINE ( 'NONE', #1762, #4557 ) ;
#3197 = DIRECTION ( 'NONE',  ( -0.000000000000000000, -1.000000000000000000, -0.000000000000000000 ) ) ;
#3198 = ADVANCED_BREP_SHAPE_REPRESENTATION ( '', ( #126, #5080 ), #3039 ) ;
#3199 = EDGE_LOOP ( 'NONE', ( #5887, #3334 ) ) ;
#3200 = VECTOR ( 'NONE', #4178, 1000.000000000000000 ) ;
#3201 = ORIENTED_EDGE ( 'NONE', *, *, #1448, .F. ) ;
#3202 = LINE ( 'NONE', #4200, #704 ) ;
#3203 = AXIS2_PLACEMENT_3D ( 'NONE', #4351, #1971, #5739 ) ;
#3204 = CARTESIAN_POINT ( 'NONE',  ( 37.50000000000000711, 6.288372600415927295E-15, 55.00000000000000000 ) ) ;
#3205 = VERTEX_POINT ( 'NONE', #1498 ) ;
#3206 = DIRECTION ( 'NONE',  ( 0.000000000000000000, 0.000000000000000000, 1.000000000000000000 ) ) ;
#3207 = CYLINDRICAL_SURFACE ( 'NONE', #223, 5.000000000000000000 ) ;
#3208 = EDGE_CURVE ( 'NONE', #2079, #1686, #3690, .T. ) ;
#3209 = EDGE_LOOP ( 'NONE', ( #5087, #5799 ) ) ;
#3210 = CARTESIAN_POINT ( 'NONE',  ( 135.4999999999999716, 8.572527594031473190E-16, 7.000000000000000000 ) ) ;
#3211 = CIRCLE ( 'NONE', #2510, 7.983406227920510467 ) ;
#3212 = ORIENTED_EDGE ( 'NONE', *, *, #567, .T. ) ;
#3213 = AXIS2_PLACEMENT_3D ( 'NONE', #1599, #4891, #2539 ) ;
#3214 = FACE_OUTER_BOUND ( 'NONE', #4629, .T. ) ;
#3215 = CARTESIAN_POINT ( 'NONE',  ( -45.00000000000001421, 40.00000000000000000, 45.00000000000000000 ) ) ;
#3216 = AXIS2_PLACEMENT_3D ( 'NONE', #3804, #5655, #5122 ) ;
#3217 = CARTESIAN_POINT ( 'NONE',  ( -49.33012701892221230, 40.00000000000000000, 37.50000000000000000 ) ) ;
#3218 = DIRECTION ( 'NONE',  ( 1.000000000000000000, 0.000000000000000000, 0.000000000000000000 ) ) ;
#3219 = CARTESIAN_POINT ( 'NONE',  ( 40.15000000000000568, 6.288372600415927295E-15, 65.00000000000000000 ) ) ;
#3220 = VERTEX_POINT ( 'NONE', #3742 ) ;
#3221 = AXIS2_PLACEMENT_3D ( 'NONE', #1536, #3188, #5043 ) ;
#3222 = FILL_AREA_STYLE_COLOUR ( '', #4202 ) ;
#3223 = AXIS2_PLACEMENT_3D ( 'NONE', #2131, #3989, #5840 ) ;
#3224 = DIRECTION ( 'NONE',  ( 1.000000000000000000, 0.000000000000000000, 0.000000000000000000 ) ) ;
#3225 = EDGE_CURVE ( 'NONE', #3927, #5326, #592, .T. ) ;
#3226 = AXIS2_PLACEMENT_3D ( 'NONE', #1777, #358, #5449 ) ;
#3228 = AXIS2_PLACEMENT_3D ( 'NONE', #4450, #328, #3990 ) ;
#3227 = DIRECTION ( 'NONE',  ( 0.000000000000000000, 0.000000000000000000, -1.000000000000000000 ) ) ;
#3229 = CARTESIAN_POINT ( 'NONE',  ( 0.000000000000000000, 0.2499999999999982792, -1.312875263449799323 ) ) ;
#3230 = AXIS2_PLACEMENT_3D ( 'NONE', #5608, #967, #3344 ) ;
#3231 = EDGE_LOOP ( 'NONE', ( #2893, #1227 ) ) ;
#3232 = ORIENTED_EDGE ( 'NONE', *, *, #4511, .F. ) ;
#3233 = DIRECTION ( 'NONE',  ( 0.4461977533474923430, -0.8949343913984144638, 0.000000000000000000 ) ) ;
#3234 = ITEM_DEFINED_TRANSFORMATION ( 'NONE', 'NONE', #5750,  #5080 ) ;
#3235 = SURFACE_STYLE_FILL_AREA ( #4656 ) ;
#3236 = ORIENTED_EDGE ( 'NONE', *, *, #1148, .T. ) ;
#3237 = CARTESIAN_POINT ( 'NONE',  ( 0.3074992278157369086, -2.196686566159251619, -2.690165171976911629E-16 ) ) ;
#3238 = DIRECTION ( 'NONE',  ( 0.8949343913984143528, 0.4461977533474922875, 0.000000000000000000 ) ) ;
#3239 = EDGE_LOOP ( 'NONE', ( #1944, #3258 ) ) ;
#3240 = ORIENTED_EDGE ( 'NONE', *, *, #2456, .F. ) ;
#3241 = AXIS2_PLACEMENT_3D ( 'NONE', #1414, #3273, #2813 ) ;
#3242 = CIRCLE ( 'NONE', #4992, 8.000000000000000000 ) ;
#3243 = FILL_AREA_STYLE ('',( #2293 ) ) ;
#3244 = CARTESIAN_POINT ( 'NONE',  ( 137.4999999999999716, 15.00000000000000000, 75.00000000000001421 ) ) ;
#3245 = CARTESIAN_POINT ( 'NONE',  ( 75.00000000000001421, -15.00000000000000355, 75.00000000000000000 ) ) ;
#3246 = CARTESIAN_POINT ( 'NONE',  ( 75.00000000000001421, 1.224646799147353207E-16, 10.49999999999999822 ) ) ;
#3247 = ORIENTED_EDGE ( 'NONE', *, *, #224, .F. ) ;
#3248 = EDGE_CURVE ( 'NONE', #4039, #1741, #925, .T. ) ;
#3249 = DIRECTION ( 'NONE',  ( 0.000000000000000000, 0.000000000000000000, -1.000000000000000000 ) ) ;
#3250 = EDGE_CURVE ( 'NONE', #1289, #5526, #5343, .T. ) ;
#3251 = CARTESIAN_POINT ( 'NONE',  ( 2.740000000000000213, 0.000000000000000000, 0.000000000000000000 ) ) ;
#3252 = EDGE_CURVE ( 'NONE', #1813, #5651, #587, .T. ) ;
#3253 = FACE_OUTER_BOUND ( 'NONE', #3763, .T. ) ;
#3254 = SHAPE_REPRESENTATION ( 'sleeve', ( #5080 ), #2647 ) ;
#3255 = ORIENTED_EDGE ( 'NONE', *, *, #1819, .T. ) ;
#3256 = PRESENTATION_STYLE_ASSIGNMENT (( #483 ) ) ;
#3257 = CARTESIAN_POINT ( 'NONE',  ( -55.00000000000001421, 40.00000000000000000, 45.00000000000000000 ) ) ;
#3258 = ORIENTED_EDGE ( 'NONE', *, *, #599, .T. ) ;
#3259 = ADVANCED_FACE ( 'NONE', ( #4213 ), #5591, .T. ) ;
#3260 = LINE ( 'NONE', #4652, #3129 ) ;
#3261 = CARTESIAN_POINT ( 'NONE',  ( 224.9999999999999716, 6.999999999999985789, 75.00000000000000000 ) ) ;
#3262 = VERTEX_POINT ( 'NONE', #3021 ) ;
#3263 = FACE_OUTER_BOUND ( 'NONE', #2850, .T. ) ;
#3264 = ORIENTED_EDGE ( 'NONE', *, *, #5393, .T. ) ;
#3265 = ORIENTED_EDGE ( 'NONE', *, *, #2208, .F. ) ;
#3266 = VECTOR ( 'NONE', #4307, 1000.000000000000000 ) ;
#3267 = DIRECTION ( 'NONE',  ( 0.000000000000000000, -0.000000000000000000, -1.000000000000000000 ) ) ;
#3268 = CARTESIAN_POINT ( 'NONE',  ( 24.99999999999998224, -6.999999999999985789, -65.00000000000000000 ) ) ;
#3269 = CARTESIAN_POINT ( 'NONE',  ( -49.33012701892221230, 40.00000000000000000, 37.50000000000000000 ) ) ;
#3270 = DIRECTION ( 'NONE',  ( -1.000000000000000000, 0.000000000000000000, -0.000000000000000000 ) ) ;
#3271 = DIRECTION ( 'NONE',  ( -0.000000000000000000, -1.000000000000000000, -0.000000000000000000 ) ) ;
#3272 = VERTEX_POINT ( 'NONE', #236 ) ;
#3273 = DIRECTION ( 'NONE',  ( 0.000000000000000000, 0.000000000000000000, 1.000000000000000000 ) ) ;
#3274 = FACE_BOUND ( 'NONE', #4241, .T. ) ;
#3275 =( REPRESENTATION_RELATIONSHIP ('NONE','NONE', #5609, #2622 ) REPRESENTATION_RELATIONSHIP_WITH_TRANSFORMATION ( #2770 )SHAPE_REPRESENTATION_RELATIONSHIP( ) );
#3276 = DIRECTION ( 'NONE',  ( 0.000000000000000000, 1.000000000000000000, 0.000000000000000000 ) ) ;
#3277 = EDGE_CURVE ( 'NONE', #4209, #782, #5911, .T. ) ;
#3278 = VERTEX_POINT ( 'NONE', #2042 ) ;
#3279 = DIRECTION ( 'NONE',  ( -0.000000000000000000, -0.000000000000000000, -1.000000000000000000 ) ) ;
#3280 = ADVANCED_FACE ( 'NONE', ( #2075, #623 ), #3415, .F. ) ;
#3281 = ORIENTED_EDGE ( 'NONE', *, *, #2719, .F. ) ;
#3282 = DIRECTION ( 'NONE',  ( 1.000000000000000000, -0.000000000000000000, -0.000000000000000000 ) ) ;
#3283 = CARTESIAN_POINT ( 'NONE',  ( 137.4999999999999716, 15.00000000000000000, -75.00000000000000000 ) ) ;
#3284 = DIRECTION ( 'NONE',  ( 0.000000000000000000, 0.000000000000000000, -1.000000000000000000 ) ) ;
#3285 = ORIENTED_EDGE ( 'NONE', *, *, #5301, .F. ) ;
#3286 = VECTOR ( 'NONE', #5151, 1000.000000000000000 ) ;
#3287 = EDGE_CURVE ( 'NONE', #2788, #4005, #3115, .T. ) ;
#3288 = CARTESIAN_POINT ( 'NONE',  ( -45.00000000000001421, 28.00000000000000355, 45.00000000000000000 ) ) ;
#3289 = VERTEX_POINT ( 'NONE', #3379 ) ;
#3290 = VERTEX_POINT ( 'NONE', #3445 ) ;
#3291 = DIRECTION ( 'NONE',  ( 0.000000000000000000, 3.490239007934759657E-15, -1.000000000000000000 ) ) ;
#3292 = CARTESIAN_POINT ( 'NONE',  ( -45.00000000000001421, 0.000000000000000000, 50.00000000000000000 ) ) ;
#3293 = CARTESIAN_POINT ( 'NONE',  ( 67.00000000000001421, 0.000000000000000000, 0.000000000000000000 ) ) ;
#3294 = DIRECTION ( 'NONE',  ( -1.000000000000000000, 0.000000000000000000, -0.000000000000000000 ) ) ;
#3295 = VECTOR ( 'NONE', #4327, 1000.000000000000000 ) ;
#3296 = PRODUCT_DEFINITION_SHAPE ( 'NONE', 'NONE',  #5973 ) ;
#3297 = CARTESIAN_POINT ( 'NONE',  ( 67.00000000000001421, 0.000000000000000000, -5.000000000000000000 ) ) ;
#3298 = AXIS2_PLACEMENT_3D ( 'NONE', #723, #246, #1570 ) ;
#3299 = ORIENTED_EDGE ( 'NONE', *, *, #3945, .T. ) ;
#3300 = DIRECTION ( 'NONE',  ( 0.000000000000000000, 0.000000000000000000, 1.000000000000000000 ) ) ;
#3301 = CARTESIAN_POINT ( 'NONE',  ( 0.06760930072668812352, 0.5150000000000032330, -0.9010842325122888630 ) ) ;
#3302 = AXIS2_PLACEMENT_3D ( 'NONE', #4331, #3507, #4909 ) ;
#3303 = DIRECTION ( 'NONE',  ( 0.000000000000000000, 1.000000000000000000, 0.000000000000000000 ) ) ;
#3304 = CARTESIAN_POINT ( 'NONE',  ( 0.05007509226404533581, 0.2499999999999982236, 1.595201548406556480 ) ) ;
#3305 = CIRCLE ( 'NONE', #2726, 4.556291390728477886 ) ;
#3306 = AXIS2_PLACEMENT_3D ( 'NONE', #3380, #3446, #2988 ) ;
#3307 = VERTEX_POINT ( 'NONE', #5361 ) ;
#3308 = DIRECTION ( 'NONE',  ( 1.000000000000000000, 0.000000000000000000, 0.000000000000000000 ) ) ;
#3309 = CIRCLE ( 'NONE', #2145, 5.000000000000004441 ) ;
#3310 = VECTOR ( 'NONE', #2657, 1000.000000000000000 ) ;
#3311 = PRODUCT_DEFINITION ( 'UNKNOWN', '', #4599, #5937 ) ;
#3312 = ORIENTED_EDGE ( 'NONE', *, *, #1842, .T. ) ;
#3313 = AXIS2_PLACEMENT_3D ( 'NONE', #4215, #57, #3294 ) ;
#3314 = CARTESIAN_POINT ( 'NONE',  ( -45.00000000000001421, 15.00000000000000000, 39.99999999999999289 ) ) ;
#3315 = CIRCLE ( 'NONE', #2832, 0.4499999999999985678 ) ;
#3316 = ADVANCED_FACE ( 'NONE', ( #680 ), #740, .F. ) ;
#3317 = DIRECTION ( 'NONE',  ( 0.000000000000000000, 0.000000000000000000, 1.000000000000000000 ) ) ;
#3318 = EDGE_CURVE ( 'NONE', #5410, #2045, #3923, .T. ) ;
#3319 =( LENGTH_UNIT ( ) NAMED_UNIT ( * ) SI_UNIT ( .MILLI., .METRE. ) );
#3320 = AXIS2_PLACEMENT_3D ( 'NONE', #3637, #2723, #4582 ) ;
#3321 = DIRECTION ( 'NONE',  ( -0.000000000000000000, -1.000000000000000000, -0.000000000000000000 ) ) ;
#3323 = ORIENTED_EDGE ( 'NONE', *, *, #3065, .T. ) ;
#3322 = EDGE_CURVE ( 'NONE', #5679, #823, #2036, .T. ) ;
#3324 = ORIENTED_EDGE ( 'NONE', *, *, #976, .F. ) ;
#3325 = CARTESIAN_POINT ( 'NONE',  ( 20.85786437626904899, 6.123233995736766282E-16, 5.000000000000000000 ) ) ;
#3326 =( GEOMETRIC_REPRESENTATION_CONTEXT ( 3 ) GLOBAL_UNCERTAINTY_ASSIGNED_CONTEXT ( ( #3784 ) ) GLOBAL_UNIT_ASSIGNED_CONTEXT ( ( #4436, #3937, #2546 ) ) REPRESENTATION_CONTEXT ( 'NONE', 'WORKASPACE' ) );
#3327 = ADVANCED_FACE ( 'NONE', ( #1101 ), #2008, .F. ) ;
#3328 = LINE ( 'NONE', #3268, #3672 ) ;
#3329 = ORIENTED_EDGE ( 'NONE', *, *, #3397, .T. ) ;
#3330 = CARTESIAN_POINT ( 'NONE',  ( -36.33974596215562514, 45.00000000000000000, 44.99999999999999289 ) ) ;
#3331 = LINE ( 'NONE', #5179, #1079 ) ;
#3332 = AXIS2_PLACEMENT_3D ( 'NONE', #1213, #3069, #5315 ) ;
#3333 = CYLINDRICAL_SURFACE ( 'NONE', #1661, 5.499999999999991118 ) ;
#3334 = ORIENTED_EDGE ( 'NONE', *, *, #2793, .F. ) ;
#3335 = ADVANCED_FACE ( 'NONE', ( #1129 ), #5270, .F. ) ;
#3336 = CARTESIAN_POINT ( 'NONE',  ( -45.00000000000001421, 50.00000000000000000, 50.00000000000000000 ) ) ;
#3337 = DIRECTION ( 'NONE',  ( -1.000000000000000000, -0.000000000000000000, -0.000000000000000000 ) ) ;
#3338 = FACE_OUTER_BOUND ( 'NONE', #1711, .T. ) ;
#3339 = VECTOR ( 'NONE', #516, 1000.000000000000000 ) ;
#3340 = ORIENTED_EDGE ( 'NONE', *, *, #5084, .F. ) ;
#3341 = ORIENTED_EDGE ( 'NONE', *, *, #5795, .T. ) ;
#3342 = CARTESIAN_POINT ( 'NONE',  ( 137.4999999999999716, 0.000000000000000000, 0.000000000000000000 ) ) ;
#3343 = EDGE_LOOP ( 'NONE', ( #1291, #1224, #2253, #5061 ) ) ;
#3344 = DIRECTION ( 'NONE',  ( 1.000000000000000000, 0.000000000000000000, 0.000000000000000000 ) ) ;
#3345 = FACE_OUTER_BOUND ( 'NONE', #2105, .T. ) ;
#3346 = PRODUCT_DEFINITION_SHAPE ( 'NONE', 'NONE',  #5982 ) ;
#3347 = LINE ( 'NONE', #1516, #3100 ) ;
#3348 = CYLINDRICAL_SURFACE ( 'NONE', #2438, 7.000000000000000000 ) ;
#3349 = ADVANCED_FACE ( 'NONE', ( #4421 ), #5300, .T. ) ;
#3350 = ORIENTED_EDGE ( 'NONE', *, *, #3094, .F. ) ;
#3351 = EDGE_CURVE ( 'NONE', #3979, #553, #4073, .T. ) ;
#3352 = ORIENTED_EDGE ( 'NONE', *, *, #3879, .T. ) ;
#3353 =( REPRESENTATION_RELATIONSHIP ('NONE','NONE', #5609, #3184 ) REPRESENTATION_RELATIONSHIP_WITH_TRANSFORMATION ( #3794 )SHAPE_REPRESENTATION_RELATIONSHIP( ) );
#3354 = CARTESIAN_POINT ( 'NONE',  ( 0.06760930072668812352, 0.5150000000000032330, -0.9010842325122888630 ) ) ;
#3355 = PRODUCT_RELATED_PRODUCT_CATEGORY ( 'part', '', ( #4115 ) ) ;
#3356 = CARTESIAN_POINT ( 'NONE',  ( 77.00000000000001421, 1.347111479062087271E-16, -8.400000000000000355 ) ) ;
#3357 = DIRECTION ( 'NONE',  ( 1.000000000000000000, 0.000000000000000000, 0.000000000000000000 ) ) ;
#3358 = DIRECTION ( 'NONE',  ( 0.4461977533474923430, -0.8949343913984144638, 0.000000000000000000 ) ) ;
#3359 = AXIS2_PLACEMENT_3D ( 'NONE', #5103, #4246, #2326 ) ;
#3360 = EDGE_LOOP ( 'NONE', ( #3559, #3666 ) ) ;
#3361 =( LENGTH_UNIT ( ) NAMED_UNIT ( * ) SI_UNIT ( .MILLI., .METRE. ) );
#3362 = CARTESIAN_POINT ( 'NONE',  ( -45.00000000000001421, 40.00000000000000000, -45.00000000000000000 ) ) ;
#3363 = CARTESIAN_POINT ( 'NONE',  ( 75.00000000000001421, 1.224646799147353207E-16, -8.500000000000000000 ) ) ;
#3364 = CARTESIAN_POINT ( 'NONE',  ( 75.00000000000001421, 0.000000000000000000, 8.500000000000000000 ) ) ;
#3365 = CARTESIAN_POINT ( 'NONE',  ( 2.740000000000000213, -0.9838866223905674557, -0.5150000000000000133 ) ) ;
#3366 = ADVANCED_FACE ( 'NONE', ( #5228, #1068, #5806 ), #4784, .F. ) ;
#3367 = ORIENTED_EDGE ( 'NONE', *, *, #2418, .T. ) ;
#3368 = VERTEX_POINT ( 'NONE', #4449 ) ;
#3369 = DIRECTION ( 'NONE',  ( 1.000000000000000000, 0.000000000000000000, 0.000000000000000000 ) ) ;
#3370 = UNCERTAINTY_MEASURE_WITH_UNIT (LENGTH_MEASURE( 1.000000000000000082E-05 ), #3076, 'distance_accuracy_value', 'NONE');
#3371 = DIRECTION ( 'NONE',  ( 0.000000000000000000, 0.000000000000000000, -1.000000000000000000 ) ) ;
#3372 = DIRECTION ( 'NONE',  ( 0.000000000000000000, 0.000000000000000000, -1.000000000000000000 ) ) ;
#3373 = CARTESIAN_POINT ( 'NONE',  ( -45.00000000000001421, 28.00000000000000355, 45.00000000000000000 ) ) ;
#3374 = ORIENTED_EDGE ( 'NONE', *, *, #2160, .F. ) ;
#3375 = ORIENTED_EDGE ( 'NONE', *, *, #3998, .F. ) ;
#3376 = CARTESIAN_POINT ( 'NONE',  ( 2.740000000000000213, 0.5150000000000035660, -0.9838866223905657904 ) ) ;
#3377 = FACE_OUTER_BOUND ( 'NONE', #5364, .T. ) ;
#3378 = ORIENTED_EDGE ( 'NONE', *, *, #97, .F. ) ;
#3379 = CARTESIAN_POINT ( 'NONE',  ( 224.9999999999999716, 6.999999999999985789, 65.00000000000000000 ) ) ;
#3380 = CARTESIAN_POINT ( 'NONE',  ( -45.00000000000001421, 50.00000000000000000, 45.00000000000000000 ) ) ;
#3381 = CARTESIAN_POINT ( 'NONE',  ( 137.4999999999999716, 7.000000000000011546, 75.00000000000001421 ) ) ;
#3382 = ORIENTED_EDGE ( 'NONE', *, *, #2254, .F. ) ;
#3383 = PRODUCT_DEFINITION ( 'UNKNOWN', '', #909, #700 ) ;
#3384 = CIRCLE ( 'NONE', #1732, 0.9999999999999991118 ) ;
#3385 = DIRECTION ( 'NONE',  ( 0.02052338132068530496, 0.000000000000000000, 0.9997893732277642886 ) ) ;
#3386 = LINE ( 'NONE', #3958, #2191 ) ;
#3387 = EDGE_CURVE ( 'NONE', #5402, #726, #4860, .T. ) ;
#3388 = CARTESIAN_POINT ( 'NONE',  ( 8.000000000000000000, -4.837354856632045452E-15, -0.5150000000000000133 ) ) ;
#3389 = VECTOR ( 'NONE', #5143, 1000.000000000000000 ) ;
#3390 = FACE_BOUND ( 'NONE', #3199, .T. ) ;
#3391 = DIRECTION ( 'NONE',  ( 0.000000000000000000, -1.224646799147353207E-16, 1.000000000000000000 ) ) ;
#3392 = PLANE ( 'NONE',  #2817 ) ;
#3393 = VERTEX_POINT ( 'NONE', #5685 ) ;
#3394 = VERTEX_POINT ( 'NONE', #1593 ) ;
#3395 = VECTOR ( 'NONE', #1281, 1000.000000000000000 ) ;
#3396 = CARTESIAN_POINT ( 'NONE',  ( -45.00000000000001421, 0.000000000000000000, 45.00000000000000000 ) ) ;
#3397 = EDGE_CURVE ( 'NONE', #4518, #1327, #5153, .T. ) ;
#3398 = VERTEX_POINT ( 'NONE', #2168 ) ;
#3399 = AXIS2_PLACEMENT_3D ( 'NONE', #1623, #4879, #1157 ) ;
#3400 = SHAPE_REPRESENTATION_RELATIONSHIP ( 'NONE' , 'NONE' ,  #5269, #1232 ) ;
#3401 = DIRECTION ( 'NONE',  ( -1.000000000000000000, -0.000000000000000000, -0.000000000000000000 ) ) ;
#3402 = CONICAL_SURFACE ( 'NONE', #4284, 0.9999999999999991118, 1.029744260000008405 ) ;
#3403 = VECTOR ( 'NONE', #629, 1000.000000000000000 ) ;
#3404 = DIRECTION ( 'NONE',  ( 0.000000000000000000, 0.000000000000000000, 1.000000000000000000 ) ) ;
#3405 = DIRECTION ( 'NONE',  ( -1.000000000000000000, -0.000000000000000000, -0.000000000000000000 ) ) ;
#3406 = VERTEX_POINT ( 'NONE', #5411 ) ;
#3407 = AXIS2_PLACEMENT_3D ( 'NONE', #2680, #1158, #4540 ) ;
#3408 = VERTEX_POINT ( 'NONE', #4539 ) ;
#3409 = CARTESIAN_POINT ( 'NONE',  ( 2.740000000000000213, -0.5149999999999973488, -0.6774776749089248540 ) ) ;
#3410 = VECTOR ( 'NONE', #1789, 1000.000000000000000 ) ;
#3411 = AXIS2_PLACEMENT_3D ( 'NONE', #1720, #365, #3636 ) ;
#3412 = AXIS2_PLACEMENT_3D ( 'NONE', #4250, #1477, #1924 ) ;
#3413 = DIRECTION ( 'NONE',  ( 1.000000000000000000, 0.000000000000000000, 0.000000000000000000 ) ) ;
#3414 = EDGE_LOOP ( 'NONE', ( #2503, #3264, #1639, #2001 ) ) ;
#3415 = PLANE ( 'NONE',  #2720 ) ;
#3416 = CARTESIAN_POINT ( 'NONE',  ( -45.00000000000001421, 40.00000000000000000, -50.00000000000000000 ) ) ;
#3417 = CARTESIAN_POINT ( 'NONE',  ( 135.4999999999999716, 0.000000000000000000, 0.000000000000000000 ) ) ;
#3418 = EDGE_LOOP ( 'NONE', ( #2590, #219, #3864, #3475 ) ) ;
#3419 = DIRECTION ( 'NONE',  ( 1.000000000000000000, 0.000000000000000000, 6.123233995736766036E-17 ) ) ;
#3420 = CARTESIAN_POINT ( 'NONE',  ( 40.15000000000000568, 6.288372600415927295E-15, 71.29999999999999716 ) ) ;
#3421 = LINE ( 'NONE', #3478, #2818 ) ;
#3422 = DIRECTION ( 'NONE',  ( 1.007709689656716815E-16, 1.153406566473941260E-16, -1.000000000000000000 ) ) ;
#3423 = FACE_OUTER_BOUND ( 'NONE', #3586, .T. ) ;
#3424 = CARTESIAN_POINT ( 'NONE',  ( 150.0000000000000284, 0.000000000000000000, -45.00000000000000000 ) ) ;
#3425 = EDGE_CURVE ( 'NONE', #5285, #4118, #3536, .T. ) ;
#3426 = ORIENTED_EDGE ( 'NONE', *, *, #130, .F. ) ;
#3427 = EDGE_CURVE ( 'NONE', #377, #3307, #2221, .T. ) ;
#3428 = ADVANCED_FACE ( 'NONE', ( #3178 ), #5386, .T. ) ;
#3429 = ORIENTED_EDGE ( 'NONE', *, *, #5552, .F. ) ;
#3430 = ORIENTED_EDGE ( 'NONE', *, *, #3018, .F. ) ;
#3431 = PRESENTATION_STYLE_ASSIGNMENT (( #5729 ) ) ;
#3432 = DIRECTION ( 'NONE',  ( 0.000000000000000000, 1.000000000000000000, 1.224646799147353207E-16 ) ) ;
#3433 = UNCERTAINTY_MEASURE_WITH_UNIT (LENGTH_MEASURE( 1.000000000000000082E-05 ), #3920, 'distance_accuracy_value', 'NONE');
#3434 = EDGE_CURVE ( 'NONE', #4908, #771, #407, .T. ) ;
#3435 = VERTEX_POINT ( 'NONE', #4971 ) ;
#3436 = CARTESIAN_POINT ( 'NONE',  ( 150.0000000000000284, 15.00000000000000000, -40.00000000000000711 ) ) ;
#3437 = PLANE ( 'NONE',  #2508 ) ;
#3438 = CLOSED_SHELL ( 'NONE', ( #4588, #1119, #1543, #3618, #429, #3349, #5794, #5866, #1968, #5839, #845, #4801, #509 ) ) ;
#3439 = CARTESIAN_POINT ( 'NONE',  ( 75.00000000000001421, 6.999999999999992006, -75.00000000000000000 ) ) ;
#3440 = VERTEX_POINT ( 'NONE', #2617 ) ;
#3441 = ADVANCED_FACE ( 'NONE', ( #5928 ), #4076, .F. ) ;
#3442 = ORIENTED_EDGE ( 'NONE', *, *, #2899, .F. ) ;
#3443 = DIRECTION ( 'NONE',  ( 0.000000000000000000, 0.000000000000000000, -1.000000000000000000 ) ) ;
#3444 = VERTEX_POINT ( 'NONE', #5030 ) ;
#3445 = CARTESIAN_POINT ( 'NONE',  ( 137.4999999999999716, -15.00000000000000000, -75.00000000000000000 ) ) ;
#3446 = DIRECTION ( 'NONE',  ( 0.000000000000000000, 1.000000000000000000, 0.000000000000000000 ) ) ;
#3447 = DIRECTION ( 'NONE',  ( 0.8949343913984144638, 0.4461977533474923430, 0.000000000000000000 ) ) ;
#3448 = ORIENTED_EDGE ( 'NONE', *, *, #4856, .F. ) ;
#3449 = DIRECTION ( 'NONE',  ( 0.000000000000000000, 0.9242245927363030855, 0.3818493186865927203 ) ) ;
#3450 = DIRECTION ( 'NONE',  ( 0.4461977533473793778, 0.8949343913984707521, -1.884057886186824495E-16 ) ) ;
#3451 = DIRECTION ( 'NONE',  ( -1.000000000000000000, -0.000000000000000000, -0.000000000000000000 ) ) ;
#3452 = CARTESIAN_POINT ( 'NONE',  ( 137.4999999999999716, 0.000000000000000000, 0.000000000000000000 ) ) ;
#3453 = DIRECTION ( 'NONE',  ( 0.8949343913984143528, -1.557891129246500526E-15, 0.4461977533474922875 ) ) ;
#3454 = LINE ( 'NONE', #2450, #3593 ) ;
#3455 = ORIENTED_EDGE ( 'NONE', *, *, #390, .F. ) ;
#3456 = AXIS2_PLACEMENT_3D ( 'NONE', #161, #1997, #3849 ) ;
#3457 = VERTEX_POINT ( 'NONE', #3591 ) ;
#3458 = SURFACE_STYLE_FILL_AREA ( #1605 ) ;
#3459 = CARTESIAN_POINT ( 'NONE',  ( -74.99999999999998579, 15.00000000000000000, 75.00000000000000000 ) ) ;
#3460 = ORIENTED_EDGE ( 'NONE', *, *, #934, .T. ) ;
#3461 = EDGE_CURVE ( 'NONE', #3160, #1679, #803, .T. ) ;
#3462 = EDGE_CURVE ( 'NONE', #5520, #2563, #5476, .T. ) ;
#3463 = CARTESIAN_POINT ( 'NONE',  ( 137.4999999999999716, 6.123233995736766282E-16, -5.000000000000000000 ) ) ;
#3464 =( REPRESENTATION_RELATIONSHIP ('NONE','NONE', #5609, #3254 ) REPRESENTATION_RELATIONSHIP_WITH_TRANSFORMATION ( #1822 )SHAPE_REPRESENTATION_RELATIONSHIP( ) );
#3465 = LINE ( 'NONE', #4291, #4464 ) ;
#3466 = ORIENTED_EDGE ( 'NONE', *, *, #3277, .F. ) ;
#3467 = ORIENTED_EDGE ( 'NONE', *, *, #39, .F. ) ;
#3468 =( NAMED_UNIT ( * ) PLANE_ANGLE_UNIT ( ) SI_UNIT ( $, .RADIAN. ) );
#3469 = ADVANCED_FACE ( 'NONE', ( #418 ), #2728, .F. ) ;
#3470 = FACE_OUTER_BOUND ( 'NONE', #1009, .T. ) ;
#3471 = ORIENTED_EDGE ( 'NONE', *, *, #2316, .F. ) ;
#3472 = DIRECTION ( 'NONE',  ( -0.000000000000000000, -1.000000000000000000, -0.000000000000000000 ) ) ;
#3473 = CARTESIAN_POINT ( 'NONE',  ( 150.0000000000000284, 0.000000000000000000, 45.00000000000000000 ) ) ;
#3474 = DIRECTION ( 'NONE',  ( 0.000000000000000000, 0.000000000000000000, -1.000000000000000000 ) ) ;
#3475 = ORIENTED_EDGE ( 'NONE', *, *, #4093, .T. ) ;
#3476 =( NAMED_UNIT ( * ) PLANE_ANGLE_UNIT ( ) SI_UNIT ( $, .RADIAN. ) );
#3477 = DIRECTION ( 'NONE',  ( 0.000000000000000000, 0.000000000000000000, 1.000000000000000000 ) ) ;
#3478 = CARTESIAN_POINT ( 'NONE',  ( 137.4999999999999716, -15.00000000000000000, -75.00000000000000000 ) ) ;
#3479 = CYLINDRICAL_SURFACE ( 'NONE', #684, 0.9999999999999991118 ) ;
#3480 = CARTESIAN_POINT ( 'NONE',  ( 25.00000000000000711, -6.999999999999988454, -65.00000000000000000 ) ) ;
#3481 = CARTESIAN_POINT ( 'NONE',  ( 2.740000000000000213, 0.9838866223910003317, 0.5149999999999999023 ) ) ;
#3482 = VECTOR ( 'NONE', #3050, 1000.000000000000000 ) ;
#3483 = ORIENTED_EDGE ( 'NONE', *, *, #1053, .F. ) ;
#3484 = AXIS2_PLACEMENT_3D ( 'NONE', #1214, #4010, #3070 ) ;
#3485 = ORIENTED_EDGE ( 'NONE', *, *, #1688, .T. ) ;
#3486 = DIRECTION ( 'NONE',  ( 0.000000000000000000, 8.673617379884040402E-17, 1.000000000000000000 ) ) ;
#3487 = AXIS2_PLACEMENT_3D ( 'NONE', #1491, #3917, #2552 ) ;
#3488 = ORIENTED_EDGE ( 'NONE', *, *, #5137, .T. ) ;
#3489 = CIRCLE ( 'NONE', #4654, 2.700000000000000178 ) ;
#3490 = VECTOR ( 'NONE', #4457, 1000.000000000000000 ) ;
#3491 = FACE_BOUND ( 'NONE', #514, .T. ) ;
#3492 = VECTOR ( 'NONE', #1865, 1000.000000000000000 ) ;
#3493 = DIRECTION ( 'NONE',  ( 1.000000000000000000, 0.000000000000000000, 0.000000000000000000 ) ) ;
#3494 = PRODUCT_DEFINITION ( 'UNKNOWN', '', #3526, #3003 ) ;
#3495 = ORIENTED_EDGE ( 'NONE', *, *, #2496, .T. ) ;
#3496 = EDGE_CURVE ( 'NONE', #1974, #5044, #4864, .T. ) ;
#3497 = ORIENTED_EDGE ( 'NONE', *, *, #2460, .F. ) ;
#3498 = AXIS2_PLACEMENT_3D ( 'NONE', #4003, #4029, #3665 ) ;
#3499 = AXIS2_PLACEMENT_3D ( 'NONE', #4308, #150, #3838 ) ;
#3500 = ADVANCED_FACE ( 'NONE', ( #5960 ), #1799, .F. ) ;
#3501 = SURFACE_STYLE_FILL_AREA ( #4933 ) ;
#3502 = CARTESIAN_POINT ( 'NONE',  ( 162.5000000000000000, 15.00000000000000000, 75.00000000000001421 ) ) ;
#3503 = VERTEX_POINT ( 'NONE', #5446 ) ;
#3504 = AXIS2_PLACEMENT_3D ( 'NONE', #2896, #4786, #4816 ) ;
#3505 = EDGE_CURVE ( 'NONE', #4824, #2304, #2823, .T. ) ;
#3506 = VECTOR ( 'NONE', #1479, 1000.000000000000000 ) ;
#3507 = DIRECTION ( 'NONE',  ( -1.000000000000000000, -0.000000000000000000, -0.000000000000000000 ) ) ;
#3508 = DIRECTION ( 'NONE',  ( 0.000000000000000000, 0.000000000000000000, -1.000000000000000000 ) ) ;
#3509 = DIRECTION ( 'NONE',  ( -0.000000000000000000, -1.000000000000000000, -0.000000000000000000 ) ) ;
#3510 = ORIENTED_EDGE ( 'NONE', *, *, #2578, .F. ) ;
#3511 = AXIS2_PLACEMENT_3D ( 'NONE', #4430, #270, #842 ) ;
#3512 = VECTOR ( 'NONE', #4221, 1000.000000000000000 ) ;
#3513 = DIRECTION ( 'NONE',  ( 0.000000000000000000, -1.000000000000000000, 0.000000000000000000 ) ) ;
#3514 = CARTESIAN_POINT ( 'NONE',  ( -49.33012701892221230, 45.00000000000000000, 37.50000000000000000 ) ) ;
#3515 = DIRECTION ( 'NONE',  ( -1.000000000000000000, 0.000000000000000000, 0.000000000000000000 ) ) ;
#3516 = CARTESIAN_POINT ( 'NONE',  ( -35.00000000000000711, 40.00000000000000000, 45.00000000000000000 ) ) ;
#3517 =( GEOMETRIC_REPRESENTATION_CONTEXT ( 3 ) GLOBAL_UNCERTAINTY_ASSIGNED_CONTEXT ( ( #3913 ) ) GLOBAL_UNIT_ASSIGNED_CONTEXT ( ( #4062, #5021, #4503 ) ) REPRESENTATION_CONTEXT ( 'NONE', 'WORKASPACE' ) );
#3518 = CARTESIAN_POINT ( 'NONE',  ( 24.99999999999998224, -7.000000000000006217, 75.00000000000000000 ) ) ;
#3519 = ORIENTED_EDGE ( 'NONE', *, *, #528, .T. ) ;
#3520 = ADVANCED_FACE ( 'NONE', ( #5864 ), #3119, .F. ) ;
#3521 =( NAMED_UNIT ( * ) PLANE_ANGLE_UNIT ( ) SI_UNIT ( $, .RADIAN. ) );
#3522 = CARTESIAN_POINT ( 'NONE',  ( 25.00000000000000711, -6.999999999999989342, 75.00000000000000000 ) ) ;
#3523 = COLOUR_RGB ( '',0.8941176470588234615, 0.8941176470588234615, 0.8941176470588234615 ) ;
#3524 = ORIENTED_EDGE ( 'NONE', *, *, #176, .T. ) ;
#3525 = SURFACE_STYLE_USAGE ( .BOTH. , #2888 ) ;
#3526 = PRODUCT_DEFINITION_FORMATION_WITH_SPECIFIED_SOURCE ( 'ANY', '', #1399, .NOT_KNOWN. ) ;
#3527 = CARTESIAN_POINT ( 'NONE',  ( 0.000000000000000000, 0.000000000000000000, 0.000000000000000000 ) ) ;
#3528 = CARTESIAN_POINT ( 'NONE',  ( 150.0000000000000284, 15.00000000000000000, -45.00000000000000000 ) ) ;
#3529 = DIRECTION ( 'NONE',  ( 0.000000000000000000, 1.000000000000000000, 0.000000000000000000 ) ) ;
#3530 = ORIENTED_EDGE ( 'NONE', *, *, #320, .F. ) ;
#3531 = VERTEX_POINT ( 'NONE', #3148 ) ;
#3532 = SURFACE_STYLE_USAGE ( .BOTH. , #765 ) ;
#3533 = ADVANCED_FACE ( 'NONE', ( #5505 ), #1339, .F. ) ;
#3534 = CLOSED_SHELL ( 'NONE', ( #5204, #23, #5947, #3335, #1270, #2302, #2806, #201, #4761, #2829, #4846, #459, #831, #70, #4707, #4355, #1275, #3500, #3316, #311, #372, #5961, #3366, #168, #646, #4955, #1024, #3441, #4997, #208, #61, #4022, #4336, #1084, #3034, #2002, #2243, #254, #4526, #3615, #2914, #5870, #2200, #5208, #1210, #2950, #4097 ) ) ;
#3535 = ORIENTED_EDGE ( 'NONE', *, *, #1526, .T. ) ;
#3536 = LINE ( 'NONE', #1709, #5441 ) ;
#3537 = CARTESIAN_POINT ( 'NONE',  ( 62.50000000000001421, -1.951563910473909559E-15, 71.29999999999999716 ) ) ;
#3538 = EDGE_CURVE ( 'NONE', #3272, #2059, #4188, .T. ) ;
#3539 = ORIENTED_EDGE ( 'NONE', *, *, #971, .T. ) ;
#3540 = CARTESIAN_POINT ( 'NONE',  ( 67.00000000000001421, 6.123233995736766282E-16, 5.000000000000000000 ) ) ;
#3541 = ORIENTED_EDGE ( 'NONE', *, *, #694, .F. ) ;
#3542 = SHAPE_DEFINITION_REPRESENTATION ( #5189, #5269 ) ;
#3543 = PRODUCT_DEFINITION ( 'UNKNOWN', '', #1189, #5455 ) ;
#3544 = CARTESIAN_POINT ( 'NONE',  ( 162.5000000000000000, 6.999999999999985789, 75.00000000000001421 ) ) ;
#3545 = CARTESIAN_POINT ( 'NONE',  ( 9.300000000000002487, 0.000000000000000000, 0.000000000000000000 ) ) ;
#3546 = CARTESIAN_POINT ( 'NONE',  ( 37.50000000000000711, 6.288372600415927295E-15, -55.00000000000000000 ) ) ;
#3547 = DIRECTION ( 'NONE',  ( 1.000000000000000000, 0.000000000000000000, 0.000000000000000000 ) ) ;
#3548 = FACE_OUTER_BOUND ( 'NONE', #3048, .T. ) ;
#3549 = VERTEX_POINT ( 'NONE', #1222 ) ;
#3550 = DIRECTION ( 'NONE',  ( -0.000000000000000000, -0.000000000000000000, 1.000000000000000000 ) ) ;
#3551 = EDGE_CURVE ( 'NONE', #1830, #2555, #3079, .T. ) ;
#3552 = ORIENTED_EDGE ( 'NONE', *, *, #907, .T. ) ;
#3553 = CARTESIAN_POINT ( 'NONE',  ( 77.00000000000001421, 1.347111479062087271E-16, 10.59999999999999787 ) ) ;
#3554 = DIRECTION ( 'NONE',  ( 0.000000000000000000, -1.000000000000000000, 0.000000000000000000 ) ) ;
#3555 = CIRCLE ( 'NONE', #4813, 0.8509999999999999787 ) ;
#3556 = AXIS2_PLACEMENT_3D ( 'NONE', #720, #5811, #657 ) ;
#3557 = CARTESIAN_POINT ( 'NONE',  ( -45.00000000000002842, 15.00000000000000000, -39.99999999999997868 ) ) ;
#3558 = ADVANCED_BREP_SHAPE_REPRESENTATION ( '', ( #2189, #5080 ), #332 ) ;
#3559 = ORIENTED_EDGE ( 'NONE', *, *, #3387, .F. ) ;
#3560 = VERTEX_POINT ( 'NONE', #5092 ) ;
#3561 = SURFACE_STYLE_USAGE ( .BOTH. , #799 ) ;
#3562 = SURFACE_SIDE_STYLE ('',( #5002 ) ) ;
#3563 = ORIENTED_EDGE ( 'NONE', *, *, #55, .T. ) ;
#3564 = DIRECTION ( 'NONE',  ( 1.000000000000000000, 0.000000000000000000, 0.000000000000000000 ) ) ;
#3565 = CARTESIAN_POINT ( 'NONE',  ( -45.00000000000001421, 40.00000000000000000, -39.99999999999999289 ) ) ;
#3566 = ORIENTED_EDGE ( 'NONE', *, *, #5334, .F. ) ;
#3567 = DIRECTION ( 'NONE',  ( 1.000000000000000000, -0.000000000000000000, -0.000000000000000000 ) ) ;
#3568 = VERTEX_POINT ( 'NONE', #4608 ) ;
#3569 = CARTESIAN_POINT ( 'NONE',  ( 3.900000000000000799, 0.000000000000000000, 2.500000000000000000 ) ) ;
#3570 = DIRECTION ( 'NONE',  ( 0.000000000000000000, 0.000000000000000000, 1.000000000000000000 ) ) ;
#3571 = LINE ( 'NONE', #5396, #1178 ) ;
#3572 = FACE_OUTER_BOUND ( 'NONE', #368, .T. ) ;
#3573 = ORIENTED_EDGE ( 'NONE', *, *, #5640, .F. ) ;
#3574 =( NAMED_UNIT ( * ) SI_UNIT ( $, .STERADIAN. ) SOLID_ANGLE_UNIT ( ) );
#3575 = EDGE_CURVE ( 'NONE', #736, #3189, #2064, .T. ) ;
#3576 = CARTESIAN_POINT ( 'NONE',  ( 67.00000000000000000, 0.000000000000000000, -9.500000000000000000 ) ) ;
#3577 = PRESENTATION_LAYER_ASSIGNMENT (  '', '', ( #188 ) ) ;
#3578 = EDGE_LOOP ( 'NONE', ( #5516, #860, #1592, #2649 ) ) ;
#3579 = APPLICATION_CONTEXT ( 'automotive_design' ) ;
#3580 = FILL_AREA_STYLE_COLOUR ( '', #2154 ) ;
#3581 = CIRCLE ( 'NONE', #1054, 2.500000000000002220 ) ;
#3582 = EDGE_CURVE ( 'NONE', #1576, #2523, #5434, .T. ) ;
#3583 = DIRECTION ( 'NONE',  ( 0.000000000000000000, -0.000000000000000000, 1.000000000000000000 ) ) ;
#3584 = AXIS2_PLACEMENT_3D ( 'NONE', #4792, #659, #2083 ) ;
#3585 = VERTEX_POINT ( 'NONE', #3237 ) ;
#3586 = EDGE_LOOP ( 'NONE', ( #595, #3098, #5860, #1003 ) ) ;
#3587 = EDGE_CURVE ( 'NONE', #2197, #3605, #4649, .T. ) ;
#3588 = FACE_OUTER_BOUND ( 'NONE', #4795, .T. ) ;
#3589 = VECTOR ( 'NONE', #4051, 1000.000000000000000 ) ;
#3590 = ORIENTED_EDGE ( 'NONE', *, *, #4836, .T. ) ;
#3591 = CARTESIAN_POINT ( 'NONE',  ( 1.299999999999999156, 0.000000000000000000, 1.000000000000000000 ) ) ;
#3592 = CARTESIAN_POINT ( 'NONE',  ( 75.00000000000001421, 6.999999999999992006, 75.00000000000000000 ) ) ;
#3593 = VECTOR ( 'NONE', #725, 1000.000000000000000 ) ;
#3594 = EDGE_LOOP ( 'NONE', ( #1372, #2329 ) ) ;
#3595 = CARTESIAN_POINT ( 'NONE',  ( 62.50000000000001421, -1.951563910473909559E-15, -65.00000000000000000 ) ) ;
#3596 = AXIS2_PLACEMENT_3D ( 'NONE', #1981, #3831, #5302 ) ;
#3597 = ORIENTED_EDGE ( 'NONE', *, *, #4048, .T. ) ;
#3598 = DIRECTION ( 'NONE',  ( 1.000000000000000000, -0.000000000000000000, -0.000000000000000000 ) ) ;
#3599 = VECTOR ( 'NONE', #625, 1000.000000000000000 ) ;
#3600 = CIRCLE ( 'NONE', #314, 7.500000000000000000 ) ;
#3601 = FACE_OUTER_BOUND ( 'NONE', #32, .T. ) ;
#3602 = LINE ( 'NONE', #5012, #4960 ) ;
#3603 = DIRECTION ( 'NONE',  ( 0.000000000000000000, 0.000000000000000000, 1.000000000000000000 ) ) ;
#3604 = PLANE ( 'NONE',  #5718 ) ;
#3605 = VERTEX_POINT ( 'NONE', #2288 ) ;
#3606 = AXIS2_PLACEMENT_3D ( 'NONE', #2781, #1892, #473 ) ;
#3607 = PLANE ( 'NONE',  #1874 ) ;
#3608 = AXIS2_PLACEMENT_3D ( 'NONE', #3643, #4994, #2671 ) ;
#3609 = STYLED_ITEM ( 'NONE', ( #4441 ), #1232 ) ;
#3610 = CONICAL_SURFACE ( 'NONE', #4092, 2.500000000000002220, 1.029744260000002631 ) ;
#3611 = ORIENTED_EDGE ( 'NONE', *, *, #4959, .T. ) ;
#3612 = ADVANCED_FACE ( 'NONE', ( #1108 ), #1076, .F. ) ;
#3613 = DIRECTION ( 'NONE',  ( -1.000000000000000000, -0.000000000000000000, -0.000000000000000000 ) ) ;
#3614 = EDGE_CURVE ( 'NONE', #4390, #1926, #5306, .T. ) ;
#3615 = ADVANCED_FACE ( 'NONE', ( #5336 ), #268, .F. ) ;
#3616 =( NAMED_UNIT ( * ) PLANE_ANGLE_UNIT ( ) SI_UNIT ( $, .RADIAN. ) );
#3617 = CYLINDRICAL_SURFACE ( 'NONE', #2743, 7.000000000000000000 ) ;
#3618 = ADVANCED_FACE ( 'NONE', ( #5691 ), #4791, .T. ) ;
#3619 = CARTESIAN_POINT ( 'NONE',  ( -25.39999999999996305, 3.061616997868383141E-16, -2.500000000000000000 ) ) ;
#3620 = PRESENTATION_LAYER_ASSIGNMENT (  '', '', ( #1386 ) ) ;
#3621 = EDGE_LOOP ( 'NONE', ( #4610, #744, #944, #2402 ) ) ;
#3622 = EDGE_LOOP ( 'NONE', ( #1316, #768, #4153, #1025 ) ) ;
#3623 = PLANE ( 'NONE',  #1579 ) ;
#3624 = AXIS2_PLACEMENT_3D ( 'NONE', #2061, #699, #1239 ) ;
#3625 = CARTESIAN_POINT ( 'NONE',  ( -40.66987298107781612, 45.00000000000000000, 37.50000000000000000 ) ) ;
#3626 = ORIENTED_EDGE ( 'NONE', *, *, #3915, .F. ) ;
#3627 = DIRECTION ( 'NONE',  ( 0.000000000000000000, 0.000000000000000000, 1.000000000000000000 ) ) ;
#3628 = EDGE_CURVE ( 'NONE', #2324, #3220, #5622, .T. ) ;
#3629 = CARTESIAN_POINT ( 'NONE',  ( -45.00000000000001421, 28.00000000000000355, 45.00000000000000000 ) ) ;
#3630 = VERTEX_POINT ( 'NONE', #4889 ) ;
#3631 = CARTESIAN_POINT ( 'NONE',  ( 172.5000000000000284, 0.000000000000000000, 0.000000000000000000 ) ) ;
#3632 = ORIENTED_EDGE ( 'NONE', *, *, #5032, .T. ) ;
#3633 = LINE ( 'NONE', #1888, #5905 ) ;
#3634 = CARTESIAN_POINT ( 'NONE',  ( -45.00000000000001421, 40.00000000000000000, -45.00000000000000000 ) ) ;
#3635 = CARTESIAN_POINT ( 'NONE',  ( -45.00000000000001421, 50.00000000000000000, 50.00000000000000000 ) ) ;
#3636 = DIRECTION ( 'NONE',  ( 1.000000000000000000, 0.000000000000000000, 0.000000000000000000 ) ) ;
#3637 = CARTESIAN_POINT ( 'NONE',  ( 0.5000000000000000000, -0.2499999999999997780, -2.000000000000000000 ) ) ;
#3638 = ORIENTED_EDGE ( 'NONE', *, *, #278, .F. ) ;
#3639 = LINE ( 'NONE', #4057, #5461 ) ;
#3640 = EDGE_LOOP ( 'NONE', ( #3853, #5019, #3103, #1801, #5789, #3014, #4719 ) ) ;
#3641 = DIRECTION ( 'NONE',  ( 0.000000000000000000, -1.000000000000000000, 0.000000000000000000 ) ) ;
#3642 = APPLICATION_PROTOCOL_DEFINITION ( 'draft international standard', 'automotive_design', 1998, #1484 ) ;
#3643 = CARTESIAN_POINT ( 'NONE',  ( 0.5477065543514070267, 0.000000000000000000, 0.000000000000000000 ) ) ;
#3644 = ADVANCED_FACE ( 'NONE', ( #5720 ), #1569, .F. ) ;
#3645 = CARTESIAN_POINT ( 'NONE',  ( -45.00000000000001421, 28.00000000000000355, 37.50000000000000000 ) ) ;
#3646 = AXIS2_PLACEMENT_3D ( 'NONE', #1326, #4528, #3192 ) ;
#3648 = EDGE_LOOP ( 'NONE', ( #3956, #3240, #4384, #4412 ) ) ;
#3647 = EDGE_CURVE ( 'NONE', #5382, #1325, #1630, .T. ) ;
#3649 = ORIENTED_EDGE ( 'NONE', *, *, #2578, .T. ) ;
#3650 = CARTESIAN_POINT ( 'NONE',  ( 0.000000000000000000, 0.000000000000000000, 75.00000000000000000 ) ) ;
#3651 = VECTOR ( 'NONE', #2937, 1000.000000000000000 ) ;
#3652 = DIRECTION ( 'NONE',  ( -1.000000000000000000, 0.000000000000000000, 0.000000000000000000 ) ) ;
#3653 = ORIENTED_EDGE ( 'NONE', *, *, #4148, .F. ) ;
#3654 = DIRECTION ( 'NONE',  ( 0.000000000000000000, 0.000000000000000000, 1.000000000000000000 ) ) ;
#3655 = DIRECTION ( 'NONE',  ( 0.000000000000000000, 1.000000000000000000, 0.000000000000000000 ) ) ;
#3656 = EDGE_LOOP ( 'NONE', ( #282, #2944 ) ) ;
#3657 = LINE ( 'NONE', #3210, #3118 ) ;
#3658 = ORIENTED_EDGE ( 'NONE', *, *, #5903, .F. ) ;
#3659 = CARTESIAN_POINT ( 'NONE',  ( 40.15000000000000568, 6.288372600415927295E-15, 71.29999999999999716 ) ) ;
#3660 = EDGE_CURVE ( 'NONE', #4439, #2598, #4400, .T. ) ;
#3661 = DIRECTION ( 'NONE',  ( -0.000000000000000000, 0.000000000000000000, 1.000000000000000000 ) ) ;
#3662 =( REPRESENTATION_RELATIONSHIP ('NONE','NONE', #5609, #2785 ) REPRESENTATION_RELATIONSHIP_WITH_TRANSFORMATION ( #47 )SHAPE_REPRESENTATION_RELATIONSHIP( ) );
#3663 = DIRECTION ( 'NONE',  ( -0.000000000000000000, -0.000000000000000000, 1.000000000000000000 ) ) ;
#3664 = DIRECTION ( 'NONE',  ( -0.000000000000000000, -0.000000000000000000, 1.000000000000000000 ) ) ;
#3665 = DIRECTION ( 'NONE',  ( 0.000000000000000000, 0.000000000000000000, -1.000000000000000000 ) ) ;
#3666 = ORIENTED_EDGE ( 'NONE', *, *, #3706, .F. ) ;
#3667 = CARTESIAN_POINT ( 'NONE',  ( 0.06760930072668894231, -0.9010842325122929708, -0.5150000000000000133 ) ) ;
#3668 = ORIENTED_EDGE ( 'NONE', *, *, #5356, .F. ) ;
#3669 = CARTESIAN_POINT ( 'NONE',  ( 2.740000000000000213, 0.5150000000000024558, -0.6774776749089207462 ) ) ;
#3670 = CARTESIAN_POINT ( 'NONE',  ( 3.900000000000000799, 0.000000000000000000, 0.000000000000000000 ) ) ;
#3671 = VERTEX_POINT ( 'NONE', #4339 ) ;
#3672 = VECTOR ( 'NONE', #3688, 1000.000000000000000 ) ;
#3673 = ORIENTED_EDGE ( 'NONE', *, *, #3755, .F. ) ;
#3674 = PLANE ( 'NONE',  #517 ) ;
#3675 = PRODUCT_CONTEXT ( 'NONE', #5027, 'mechanical' ) ;
#3676 = PRESENTATION_LAYER_ASSIGNMENT (  '', '', ( #293 ) ) ;
#3677 = CARTESIAN_POINT ( 'NONE',  ( 0.5000000000000000000, 0.000000000000000000, 0.000000000000000000 ) ) ;
#3678 = ORIENTED_EDGE ( 'NONE', *, *, #4602, .T. ) ;
#3679 = DIRECTION ( 'NONE',  ( 0.000000000000000000, -1.000000000000000000, 0.000000000000000000 ) ) ;
#3680 = CARTESIAN_POINT ( 'NONE',  ( 35.00000000000000000, 6.288372600415927295E-15, -55.00000000000000000 ) ) ;
#3681 = EDGE_CURVE ( 'NONE', #2045, #3290, #3421, .T. ) ;
#3682 = EDGE_LOOP ( 'NONE', ( #1265, #261 ) ) ;
#3683 = EDGE_CURVE ( 'NONE', #3549, #1773, #1134, .T. ) ;
#3684 = ORIENTED_EDGE ( 'NONE', *, *, #1410, .T. ) ;
#3685 = AXIS2_PLACEMENT_3D ( 'NONE', #2646, #2187, #4961 ) ;
#3686 = CARTESIAN_POINT ( 'NONE',  ( -45.00000000000001421, 40.00000000000000000, 39.99999999999999289 ) ) ;
#3687 = EDGE_CURVE ( 'NONE', #1480, #3012, #591, .T. ) ;
#3688 = DIRECTION ( 'NONE',  ( -1.000000000000000000, 0.000000000000000000, 0.000000000000000000 ) ) ;
#3689 =( GEOMETRIC_REPRESENTATION_CONTEXT ( 3 ) GLOBAL_UNCERTAINTY_ASSIGNED_CONTEXT ( ( #1051 ) ) GLOBAL_UNIT_ASSIGNED_CONTEXT ( ( #556, #4235, #1913 ) ) REPRESENTATION_CONTEXT ( 'NONE', 'WORKASPACE' ) );
#3690 = CIRCLE ( 'NONE', #2135, 1.099999999999998535 ) ;
#3691 = DIRECTION ( 'NONE',  ( -0.8660254037844384856, 0.000000000000000000, 0.5000000000000004441 ) ) ;
#3692 = FACE_OUTER_BOUND ( 'NONE', #2588, .T. ) ;
#3693 = LINE ( 'NONE', #4271, #4863 ) ;
#3694 = ORIENTED_EDGE ( 'NONE', *, *, #1389, .F. ) ;
#3695 = AXIS2_PLACEMENT_3D ( 'NONE', #3481, #2476, #182 ) ;
#3696 =( NAMED_UNIT ( * ) SI_UNIT ( $, .STERADIAN. ) SOLID_ANGLE_UNIT ( ) );
#3697 = AXIS2_PLACEMENT_3D ( 'NONE', #1980, #5710, #3830 ) ;
#3698 = DIRECTION ( 'NONE',  ( 0.000000000000000000, 0.000000000000000000, 1.000000000000000000 ) ) ;
#3699 = AXIS2_PLACEMENT_3D ( 'NONE', #3631, #2198, #4543 ) ;
#3701 = AXIS2_PLACEMENT_3D ( 'NONE', #5532, #1376, #4205 ) ;
#3700 = DIRECTION ( 'NONE',  ( -0.000000000000000000, -0.000000000000000000, -1.000000000000000000 ) ) ;
#3702 = EDGE_CURVE ( 'NONE', #105, #1147, #1559, .T. ) ;
#3703 = AXIS2_PLACEMENT_3D ( 'NONE', #485, #2330, #912 ) ;
#3704 = DIRECTION ( 'NONE',  ( 0.8949343913984707521, 0.000000000000000000, -0.4461977533473793223 ) ) ;
#3705 = AXIS2_PLACEMENT_3D ( 'NONE', #3099, #4954, #1787 ) ;
#3706 = EDGE_CURVE ( 'NONE', #726, #5402, #1850, .T. ) ;
#3707 =( GEOMETRIC_REPRESENTATION_CONTEXT ( 3 ) GLOBAL_UNCERTAINTY_ASSIGNED_CONTEXT ( ( #4829 ) ) GLOBAL_UNIT_ASSIGNED_CONTEXT ( ( #2155, #5377, #3943 ) ) REPRESENTATION_CONTEXT ( 'NONE', 'WORKASPACE' ) );
#3708 = VERTEX_POINT ( 'NONE', #4427 ) ;
#3709 = CARTESIAN_POINT ( 'NONE',  ( 0.000000000000000000, 0.000000000000000000, -75.00000000000000000 ) ) ;
#3710 = PRODUCT_CONTEXT ( 'NONE', #4520, 'mechanical' ) ;
#3711 =( GEOMETRIC_REPRESENTATION_CONTEXT ( 3 ) GLOBAL_UNCERTAINTY_ASSIGNED_CONTEXT ( ( #573 ) ) GLOBAL_UNIT_ASSIGNED_CONTEXT ( ( #1086, #3037, #2574 ) ) REPRESENTATION_CONTEXT ( 'NONE', 'WORKASPACE' ) );
#3712 = DIRECTION ( 'NONE',  ( -1.000000000000000000, -0.000000000000000000, -0.000000000000000000 ) ) ;
#3713 = ORIENTED_EDGE ( 'NONE', *, *, #3902, .F. ) ;
#3714 = CARTESIAN_POINT ( 'NONE',  ( 224.9999999999999716, 6.999999999999985789, 75.00000000000000000 ) ) ;
#3715 = ORIENTED_EDGE ( 'NONE', *, *, #1451, .T. ) ;
#3716 = AXIS2_PLACEMENT_3D ( 'NONE', #1447, #3369, #545 ) ;
#3717 = VERTEX_POINT ( 'NONE', #3060 ) ;
#3718 = ORIENTED_EDGE ( 'NONE', *, *, #4697, .T. ) ;
#3719 = DIRECTION ( 'NONE',  ( 0.000000000000000000, 0.000000000000000000, -1.000000000000000000 ) ) ;
#3720 = ADVANCED_FACE ( 'NONE', ( #4917, #2082, #2014 ), #747, .F. ) ;
#3721 = CARTESIAN_POINT ( 'NONE',  ( 24.99999999999998224, 6.999999999999985789, 65.00000000000000000 ) ) ;
#3722 = CARTESIAN_POINT ( 'NONE',  ( 1.314929834301322591E-16, 0.000000000000000000, 0.000000000000000000 ) ) ;
#3723 = FACE_OUTER_BOUND ( 'NONE', #5407, .T. ) ;
#3724 = ORIENTED_EDGE ( 'NONE', *, *, #5293, .F. ) ;
#3725 = EDGE_CURVE ( 'NONE', #1037, #4171, #4820, .T. ) ;
#3726 = DIRECTION ( 'NONE',  ( 0.000000000000000000, 0.000000000000000000, 1.000000000000000000 ) ) ;
#3727 = CARTESIAN_POINT ( 'NONE',  ( -74.99999999999998579, -15.00000000000000000, 75.00000000000000000 ) ) ;
#3728 = DIRECTION ( 'NONE',  ( -1.000000000000000000, -4.770489558936220126E-17, 0.000000000000000000 ) ) ;
#3729 = EDGE_LOOP ( 'NONE', ( #5626, #2192, #1589 ) ) ;
#3730 = APPLICATION_PROTOCOL_DEFINITION ( 'draft international standard', 'automotive_design', 1998, #1797 ) ;
#3731 = CARTESIAN_POINT ( 'NONE',  ( 0.5000000000000000000, 0.2499999999999982792, 2.000000000000001776 ) ) ;
#3732 = ADVANCED_FACE ( 'NONE', ( #3897 ), #4751, .F. ) ;
#3733 = ORIENTED_EDGE ( 'NONE', *, *, #2278, .T. ) ;
#3734 = DIRECTION ( 'NONE',  ( 0.000000000000000000, 1.000000000000000000, -0.000000000000000000 ) ) ;
#3735 = PLANE ( 'NONE',  #3910 ) ;
#3736 = ORIENTED_EDGE ( 'NONE', *, *, #333, .T. ) ;
#3737 = DIRECTION ( 'NONE',  ( 0.000000000000000000, 0.000000000000000000, 1.000000000000000000 ) ) ;
#3738 = ORIENTED_EDGE ( 'NONE', *, *, #2496, .F. ) ;
#3739 = VERTEX_POINT ( 'NONE', #1039 ) ;
#3740 = CARTESIAN_POINT ( 'NONE',  ( 37.50000000000000711, 6.288372600415927295E-15, 71.29999999999999716 ) ) ;
#3741 = CARTESIAN_POINT ( 'NONE',  ( 75.00000000000001421, 0.000000000000000000, -9.500000000000000000 ) ) ;
#3742 = CARTESIAN_POINT ( 'NONE',  ( 0.3226060873438244547, -2.189154565102686245, -0.5150000000000000133 ) ) ;
#3743 = DIRECTION ( 'NONE',  ( 0.000000000000000000, 0.000000000000000000, 1.000000000000000000 ) ) ;
#3744 = DIRECTION ( 'NONE',  ( 0.000000000000000000, 0.000000000000000000, -1.000000000000000000 ) ) ;
#3745 = VERTEX_POINT ( 'NONE', #2442 ) ;
#3746 = DIRECTION ( 'NONE',  ( 1.000000000000000000, 0.000000000000000000, 0.000000000000000000 ) ) ;
#3747 = CYLINDRICAL_SURFACE ( 'NONE', #4429, 5.000000000000004441 ) ;
#3748 = CARTESIAN_POINT ( 'NONE',  ( 196.6421356237309510, 0.000000000000000000, 0.000000000000000000 ) ) ;
#3749 = CARTESIAN_POINT ( 'NONE',  ( 55.00000000000000711, 6.123233995736766282E-16, -5.000000000000000000 ) ) ;
#3750 = EDGE_CURVE ( 'NONE', #4296, #2304, #144, .T. ) ;
#3751 = ORIENTED_EDGE ( 'NONE', *, *, #5422, .T. ) ;
#3752 = SURFACE_SIDE_STYLE ('',( #1001 ) ) ;
#3753 = FACE_OUTER_BOUND ( 'NONE', #4233, .T. ) ;
#3754 = ADVANCED_FACE ( 'NONE', ( #1130 ), #1594, .F. ) ;
#3755 = EDGE_CURVE ( 'NONE', #2954, #105, #5711, .T. ) ;
#3756 = VERTEX_POINT ( 'NONE', #2043 ) ;
#3757 = DIRECTION ( 'NONE',  ( -1.000000000000000000, -0.000000000000000000, -0.000000000000000000 ) ) ;
#3758 = DIRECTION ( 'NONE',  ( -1.000000000000000000, -0.000000000000000000, -0.000000000000000000 ) ) ;
#3759 = VECTOR ( 'NONE', #2615, 1000.000000000000000 ) ;
#3760 = CARTESIAN_POINT ( 'NONE',  ( 40.00000000000000711, 6.594534300202765954E-15, -65.00000000000000000 ) ) ;
#3761 = ORIENTED_EDGE ( 'NONE', *, *, #2425, .F. ) ;
#3762 = EDGE_CURVE ( 'NONE', #3393, #4227, #2041, .T. ) ;
#3763 = EDGE_LOOP ( 'NONE', ( #3483, #4871, #5166, #3940, #2074, #752, #5198, #3378, #773, #409, #3824, #5635, #5065 ) ) ;
#3764 = PRESENTATION_LAYER_ASSIGNMENT (  '', '', ( #394 ) ) ;
#3765 = CIRCLE ( 'NONE', #3484, 5.000000000000004441 ) ;
#3766 = DIRECTION ( 'NONE',  ( 1.000000000000000000, 0.000000000000000000, 0.000000000000000000 ) ) ;
#3767 = ORIENTED_EDGE ( 'NONE', *, *, #5078, .F. ) ;
#3768 = CARTESIAN_POINT ( 'NONE',  ( 75.00000000000001421, 0.000000000000000000, 9.500000000000000000 ) ) ;
#3769 = LINE ( 'NONE', #4239, #701 ) ;
#3770 = PRODUCT_DEFINITION_SHAPE ( 'NONE', 'NONE',  #2413 ) ;
#3771 = CARTESIAN_POINT ( 'NONE',  ( -53.66025403784439618, 45.00000000000000000, 45.00000000000001421 ) ) ;
#3772 = EDGE_LOOP ( 'NONE', ( #4998, #44, #5535, #4796 ) ) ;
#3773 = B_SPLINE_CURVE_WITH_KNOTS ( 'NONE', 3,
 ( #772, #806, #2621, #1712, #330, #5414 ),
 .UNSPECIFIED., .F., .F.,
 ( 4, 2, 4 ),
 ( 0.003549988921687060456, 0.003971677118101641160, 0.004393365314516220997 ),
 .UNSPECIFIED. ) ;
#3774 = FILL_AREA_STYLE_COLOUR ( '', #1678 ) ;
#3775 = CARTESIAN_POINT ( 'NONE',  ( -45.00000000000001421, 30.00000000000000355, 37.50000000000000000 ) ) ;
#3776 = VECTOR ( 'NONE', #1231, 1000.000000000000000 ) ;
#3777 = CARTESIAN_POINT ( 'NONE',  ( 162.5000000000000000, 15.00000000000000000, 75.00000000000001421 ) ) ;
#3778 = PLANE ( 'NONE',  #2641 ) ;
#3779 = ORIENTED_EDGE ( 'NONE', *, *, #3791, .T. ) ;
#3780 = AXIS2_PLACEMENT_3D ( 'NONE', #2322, #1839, #534 ) ;
#3781 = VECTOR ( 'NONE', #2538, 1000.000000000000000 ) ;
#3782 = VERTEX_POINT ( 'NONE', #4785 ) ;
#3783 = CARTESIAN_POINT ( 'NONE',  ( 3.900000000000000799, 0.000000000000000000, 0.000000000000000000 ) ) ;
#3784 = UNCERTAINTY_MEASURE_WITH_UNIT (LENGTH_MEASURE( 1.000000000000000082E-05 ), #4436, 'distance_accuracy_value', 'NONE');
#3785 = EDGE_CURVE ( 'NONE', #1708, #1426, #5686, .T. ) ;
#3786 = AXIS2_PLACEMENT_3D ( 'NONE', #5281, #2475, #181 ) ;
#3787 = CIRCLE ( 'NONE', #4771, 5.000000000000000000 ) ;
#3788 = EDGE_CURVE ( 'NONE', #5323, #5481, #237, .T. ) ;
#3789 = ORIENTED_EDGE ( 'NONE', *, *, #3683, .F. ) ;
#3790 = CARTESIAN_POINT ( 'NONE',  ( 2.740000000000000213, 0.000000000000000000, 0.000000000000000000 ) ) ;
#3791 = EDGE_CURVE ( 'NONE', #1680, #4352, #5915, .T. ) ;
#3792 = AXIS2_PLACEMENT_3D ( 'NONE', #1080, #249, #2017 ) ;
#3793 = LINE ( 'NONE', #5218, #4326 ) ;
#3794 = ITEM_DEFINED_TRANSFORMATION ( 'NONE', 'NONE', #4104,  #5080 ) ;
#3795 = DIRECTION ( 'NONE',  ( -1.000000000000000000, 0.000000000000000000, 0.000000000000000000 ) ) ;
#3796 = CIRCLE ( 'NONE', #1767, 4.999999999999990230 ) ;
#3797 =( NAMED_UNIT ( * ) SI_UNIT ( $, .STERADIAN. ) SOLID_ANGLE_UNIT ( ) );
#3798 = EDGE_LOOP ( 'NONE', ( #1928, #3909, #5892, #679 ) ) ;
#3799 = ORIENTED_EDGE ( 'NONE', *, *, #4697, .F. ) ;
#3800 = DIRECTION ( 'NONE',  ( 0.000000000000000000, -3.491481338843133355E-15, 1.000000000000000000 ) ) ;
#3801 = EDGE_CURVE ( 'NONE', #128, #1155, #4842, .T. ) ;
#3802 = DIRECTION ( 'NONE',  ( 0.4461977533473793778, 0.8949343913984707521, -1.884057886186824495E-16 ) ) ;
#3803 = ORIENTED_EDGE ( 'NONE', *, *, #4249, .T. ) ;
#3804 = CARTESIAN_POINT ( 'NONE',  ( -45.00000000000001421, 50.00000000000000000, 45.00000000000000000 ) ) ;
#3805 = DIRECTION ( 'NONE',  ( 0.000000000000000000, 0.000000000000000000, -1.000000000000000000 ) ) ;
#3806 = AXIS2_PLACEMENT_3D ( 'NONE', #4640, #477, #4363 ) ;
#3807 = LINE ( 'NONE', #716, #3599 ) ;
#3808 = ORIENTED_EDGE ( 'NONE', *, *, #4277, .F. ) ;
#3809 = CARTESIAN_POINT ( 'NONE',  ( 0.000000000000000000, 84.99999999999998579, 0.000000000000000000 ) ) ;
#3810 = CYLINDRICAL_SURFACE ( 'NONE', #361, 5.000000000000004441 ) ;
#3811 = CARTESIAN_POINT ( 'NONE',  ( 75.00000000000001421, 8.572527594031473190E-16, 7.000000000000000000 ) ) ;
#3812 = FACE_OUTER_BOUND ( 'NONE', #154, .T. ) ;
#3813 = CARTESIAN_POINT ( 'NONE',  ( -45.00000000000001421, 0.000000000000000000, 45.00000000000000000 ) ) ;
#3814 = ORIENTED_EDGE ( 'NONE', *, *, #5105, .F. ) ;
#3815 = ORIENTED_EDGE ( 'NONE', *, *, #5912, .F. ) ;
#3816 =( LENGTH_UNIT ( ) NAMED_UNIT ( * ) SI_UNIT ( .MILLI., .METRE. ) );
#3817 = LINE ( 'NONE', #5250, #1585 ) ;
#3818 = EDGE_CURVE ( 'NONE', #1680, #4908, #5229, .T. ) ;
#3819 = VERTEX_POINT ( 'NONE', #4269 ) ;
#3820 = DIRECTION ( 'NONE',  ( -0.000000000000000000, -1.000000000000000000, -0.000000000000000000 ) ) ;
#3821 = CARTESIAN_POINT ( 'NONE',  ( 62.50000000000001421, -1.951563910473909559E-15, 53.49784845693390167 ) ) ;
#3822 = CARTESIAN_POINT ( 'NONE',  ( 2.740000000000000213, 0.9838866223910001096, -0.5150000000000001243 ) ) ;
#3823 = DIRECTION ( 'NONE',  ( 0.000000000000000000, 0.000000000000000000, 1.000000000000000000 ) ) ;
#3824 = ORIENTED_EDGE ( 'NONE', *, *, #405, .F. ) ;
#3825 = ORIENTED_EDGE ( 'NONE', *, *, #4438, .T. ) ;
#3826 = EDGE_CURVE ( 'NONE', #939, #2126, #2468, .T. ) ;
#3827 = CARTESIAN_POINT ( 'NONE',  ( -45.00000000000001421, 30.00000000000000355, -45.00000000000000000 ) ) ;
#3828 = CARTESIAN_POINT ( 'NONE',  ( 0.000000000000000000, -2.349999999999997424, 0.5149999999999992362 ) ) ;
#3829 = ORIENTED_EDGE ( 'NONE', *, *, #1490, .T. ) ;
#3830 = DIRECTION ( 'NONE',  ( 0.000000000000000000, 0.000000000000000000, -1.000000000000000000 ) ) ;
#3831 = DIRECTION ( 'NONE',  ( -0.000000000000000000, -0.000000000000000000, -1.000000000000000000 ) ) ;
#3832 = DIRECTION ( 'NONE',  ( 0.000000000000000000, 0.000000000000000000, -1.000000000000000000 ) ) ;
#3833 = CIRCLE ( 'NONE', #3646, 7.983406227920510467 ) ;
#3834 = ORIENTED_EDGE ( 'NONE', *, *, #3785, .F. ) ;
#3835 = EDGE_CURVE ( 'NONE', #4118, #2775, #1950, .T. ) ;
#3836 = PRODUCT_CONTEXT ( 'NONE', #5751, 'mechanical' ) ;
#3837 = DIRECTION ( 'NONE',  ( -0.8571673013836870192, 1.049727191973306873E-16, 0.5150380737757234151 ) ) ;
#3838 = DIRECTION ( 'NONE',  ( 0.000000000000000000, -0.000000000000000000, 1.000000000000000000 ) ) ;
#3839 = LINE ( 'NONE', #3363, #4068 ) ;
#3840 = CARTESIAN_POINT ( 'NONE',  ( 43.00000000000000000, 6.288372600415927295E-15, 75.00000000000000000 ) ) ;
#3841 = CARTESIAN_POINT ( 'NONE',  ( 40.00000000000000711, 6.288372600415927295E-15, 55.00000000000000000 ) ) ;
#3842 = ORIENTED_EDGE ( 'NONE', *, *, #793, .F. ) ;
#3843 = ORIENTED_EDGE ( 'NONE', *, *, #3941, .F. ) ;
#3844 = SHAPE_REPRESENTATION_RELATIONSHIP ( 'NONE' , 'NONE' ,  #3254, #4722 ) ;
#3845 = DIRECTION ( 'NONE',  ( 1.000000000000000000, 0.000000000000000000, 0.000000000000000000 ) ) ;
#3846 = UNCERTAINTY_MEASURE_WITH_UNIT (LENGTH_MEASURE( 1.000000000000000082E-05 ), #3319, 'distance_accuracy_value', 'NONE');
#3847 = ORIENTED_EDGE ( 'NONE', *, *, #4048, .F. ) ;
#3848 = CARTESIAN_POINT ( 'NONE',  ( 150.0000000000000284, 0.000000000000000000, -45.00000000000000000 ) ) ;
#3849 = DIRECTION ( 'NONE',  ( 0.000000000000000000, 0.000000000000000000, 1.000000000000000000 ) ) ;
#3850 = DIRECTION ( 'NONE',  ( -1.000000000000000000, 0.000000000000000000, 0.000000000000000000 ) ) ;
#3851 =( LENGTH_UNIT ( ) NAMED_UNIT ( * ) SI_UNIT ( .MILLI., .METRE. ) );
#3852 = VERTEX_POINT ( 'NONE', #1625 ) ;
#3853 = ORIENTED_EDGE ( 'NONE', *, *, #5321, .F. ) ;
#3854 = DIRECTION ( 'NONE',  ( -1.000000000000000000, -0.000000000000000000, -0.000000000000000000 ) ) ;
#3855 = AXIS2_PLACEMENT_3D ( 'NONE', #3950, #2490, #4299 ) ;
#3856 = DIRECTION ( 'NONE',  ( 1.007709689656716815E-16, 1.153406566473941260E-16, -1.000000000000000000 ) ) ;
#3857 = ADVANCED_FACE ( 'NONE', ( #3924, #2009, #202 ), #3861, .F. ) ;
#3858 = EDGE_LOOP ( 'NONE', ( #4639, #1423, #3519, #3825 ) ) ;
#3859 = CARTESIAN_POINT ( 'NONE',  ( -35.00000000000000711, 40.00000000000000000, 45.00000000000000000 ) ) ;
#3860 = ADVANCED_FACE ( 'NONE', ( #2961 ), #2493, .T. ) ;
#3861 = PLANE ( 'NONE',  #2924 ) ;
#3862 = EDGE_CURVE ( 'NONE', #3205, #4999, #2048, .T. ) ;
#3863 = DIRECTION ( 'NONE',  ( 0.8949343913984144638, 0.4461977533474923430, 0.000000000000000000 ) ) ;
#3864 = ORIENTED_EDGE ( 'NONE', *, *, #3628, .T. ) ;
#3865 = VECTOR ( 'NONE', #5028, 1000.000000000000114 ) ;
#3866 = ADVANCED_FACE ( 'NONE', ( #1499 ), #27, .T. ) ;
#3867 = CARTESIAN_POINT ( 'NONE',  ( 62.50000000000001421, -1.951563910473909559E-15, 65.00000000000000000 ) ) ;
#3868 = CARTESIAN_POINT ( 'NONE',  ( 37.50000000000000711, 6.288372600415927295E-15, -65.00000000000000000 ) ) ;
#3869 = AXIS2_PLACEMENT_3D ( 'NONE', #4663, #2777, #3183 ) ;
#3870 = CIRCLE ( 'NONE', #1650, 5.000000000000000000 ) ;
#3871 = CARTESIAN_POINT ( 'NONE',  ( -36.33974596215562514, 40.00000000000000000, 44.99999999999999289 ) ) ;
#3872 = CYLINDRICAL_SURFACE ( 'NONE', #1668, 5.000000000000004441 ) ;
#3873 = LINE ( 'NONE', #4893, #1672 ) ;
#3874 = EDGE_LOOP ( 'NONE', ( #4834, #5576 ) ) ;
#3875 = DIRECTION ( 'NONE',  ( 1.000000000000000000, 0.000000000000000000, 0.000000000000000000 ) ) ;
#3876 = FILL_AREA_STYLE ('',( #5286 ) ) ;
#3877 = VECTOR ( 'NONE', #1703, 1000.000000000000000 ) ;
#3878 = DIRECTION ( 'NONE',  ( -0.000000000000000000, -0.000000000000000000, -1.000000000000000000 ) ) ;
#3879 = EDGE_CURVE ( 'NONE', #3394, #5618, #4192, .T. ) ;
#3880 = EDGE_LOOP ( 'NONE', ( #1803, #1365 ) ) ;
#3881 = AXIS2_PLACEMENT_3D ( 'NONE', #4053, #2272, #1235 ) ;
#3882 = AXIS2_PLACEMENT_3D ( 'NONE', #2295, #5073, #2664 ) ;
#3883 = SURFACE_STYLE_FILL_AREA ( #2065 ) ;
#3884 = FACE_OUTER_BOUND ( 'NONE', #4962, .T. ) ;
#3885 = CIRCLE ( 'NONE', #1271, 5.000000000000004441 ) ;
#3886 = AXIS2_PLACEMENT_3D ( 'NONE', #2406, #5748, #4726 ) ;
#3887 = APPLICATION_CONTEXT ( 'automotive_design' ) ;
#3888 = DIRECTION ( 'NONE',  ( 1.000000000000000000, -3.469446951953614189E-16, -0.000000000000000000 ) ) ;
#3889 = ORIENTED_EDGE ( 'NONE', *, *, #233, .T. ) ;
#3890 = VECTOR ( 'NONE', #2222, 1000.000000000000000 ) ;
#3891 = EDGE_LOOP ( 'NONE', ( #192, #5076, #2087, #664, #1313 ) ) ;
#3892 = VECTOR ( 'NONE', #549, 1000.000000000000000 ) ;
#3893 = VECTOR ( 'NONE', #3613, 1000.000000000000000 ) ;
#3894 = CARTESIAN_POINT ( 'NONE',  ( 77.00000000000001421, 0.000000000000000000, 0.000000000000000000 ) ) ;
#3895 = ORIENTED_EDGE ( 'NONE', *, *, #4507, .F. ) ;
#3896 = CARTESIAN_POINT ( 'NONE',  ( 19.70000000000000284, 0.000000000000000000, 0.000000000000000000 ) ) ;
#3897 = FACE_OUTER_BOUND ( 'NONE', #487, .T. ) ;
#3898 = DIRECTION ( 'NONE',  ( 0.000000000000000000, 1.000000000000000000, 1.086455722314322026E-16 ) ) ;
#3899 = VERTEX_POINT ( 'NONE', #1223 ) ;
#3900 = CARTESIAN_POINT ( 'NONE',  ( 122.5000000000000142, -22.64068087405963325, -59.47604197959874028 ) ) ;
#3901 = CARTESIAN_POINT ( 'NONE',  ( 2.740000000000000213, 0.6774776749089228556, 0.5149999999999997913 ) ) ;
#3902 = EDGE_CURVE ( 'NONE', #1345, #702, #1685, .T. ) ;
#3903 = CARTESIAN_POINT ( 'NONE',  ( 0.06760930072668799862, 0.5149999999999969047, 0.9010842325122926377 ) ) ;
#3904 = AXIS2_PLACEMENT_3D ( 'NONE', #3809, #3249, #5659 ) ;
#3905 = DIRECTION ( 'NONE',  ( 1.000000000000000000, 0.000000000000000000, 0.000000000000000000 ) ) ;
#3906 = CARTESIAN_POINT ( 'NONE',  ( 60.00000000000001421, -1.951563910473909559E-15, -65.00000000000000000 ) ) ;
#3907 = EDGE_CURVE ( 'NONE', #5326, #5390, #5447, .T. ) ;
#3908 = CARTESIAN_POINT ( 'NONE',  ( 0.6000000000000000888, 0.000000000000000000, 0.000000000000000000 ) ) ;
#3909 = ORIENTED_EDGE ( 'NONE', *, *, #1419, .F. ) ;
#3910 = AXIS2_PLACEMENT_3D ( 'NONE', #5057, #5583, #4071 ) ;
#3911 = ORIENTED_EDGE ( 'NONE', *, *, #4621, .F. ) ;
#3912 = LINE ( 'NONE', #3459, #2077 ) ;
#3913 = UNCERTAINTY_MEASURE_WITH_UNIT (LENGTH_MEASURE( 1.000000000000000082E-05 ), #4062, 'distance_accuracy_value', 'NONE');
#3914 = VERTEX_POINT ( 'NONE', #5865 ) ;
#3915 = EDGE_CURVE ( 'NONE', #4390, #128, #263, .T. ) ;
#3916 = CARTESIAN_POINT ( 'NONE',  ( 34.85000000000000853, 6.612904002189975595E-15, 71.29999999999999716 ) ) ;
#3917 = DIRECTION ( 'NONE',  ( 1.000000000000000000, 0.000000000000000000, 0.000000000000000000 ) ) ;
#3918 = ORIENTED_EDGE ( 'NONE', *, *, #755, .F. ) ;
#3919 = ORIENTED_EDGE ( 'NONE', *, *, #562, .T. ) ;
#3920 =( LENGTH_UNIT ( ) NAMED_UNIT ( * ) SI_UNIT ( .MILLI., .METRE. ) );
#3921 = DIRECTION ( 'NONE',  ( -0.000000000000000000, -1.000000000000000000, -0.000000000000000000 ) ) ;
#3922 = ORIENTED_EDGE ( 'NONE', *, *, #5615, .F. ) ;
#3923 = LINE ( 'NONE', #4814, #3976 ) ;
#3924 = FACE_BOUND ( 'NONE', #1283, .T. ) ;
#3925 = VECTOR ( 'NONE', #3758, 1000.000000000000000 ) ;
#3926 = DIRECTION ( 'NONE',  ( 1.000000000000000000, -0.000000000000000000, -0.000000000000000000 ) ) ;
#3927 = VERTEX_POINT ( 'NONE', #3592 ) ;
#3928 = PRODUCT_CONTEXT ( 'NONE', #2653, 'mechanical' ) ;
#3929 = FACE_OUTER_BOUND ( 'NONE', #2170, .T. ) ;
#3930 = DIRECTION ( 'NONE',  ( 0.8660254037844393737, -0.000000000000000000, 0.4999999999999987232 ) ) ;
#3931 = CARTESIAN_POINT ( 'NONE',  ( 137.4999999999999716, 0.000000000000000000, 0.000000000000000000 ) ) ;
#3932 = DIRECTION ( 'NONE',  ( 0.000000000000000000, 0.000000000000000000, 1.000000000000000000 ) ) ;
#3933 = CARTESIAN_POINT ( 'NONE',  ( 0.000000000000000000, -2.349999999999999201, 0.5149999999999992362 ) ) ;
#3934 = VERTEX_POINT ( 'NONE', #2132 ) ;
#3935 = VECTOR ( 'NONE', #3008, 1000.000000000000000 ) ;
#3936 = ORIENTED_EDGE ( 'NONE', *, *, #3687, .T. ) ;
#3937 =( NAMED_UNIT ( * ) PLANE_ANGLE_UNIT ( ) SI_UNIT ( $, .RADIAN. ) );
#3938 = DIRECTION ( 'NONE',  ( 0.000000000000000000, 1.000000000000000000, 0.000000000000000000 ) ) ;
#3939 = PRODUCT_DEFINITION ( 'UNKNOWN', '', #4009, #4410 ) ;
#3940 = ORIENTED_EDGE ( 'NONE', *, *, #280, .T. ) ;
#3941 = EDGE_CURVE ( 'NONE', #2650, #2749, #2525, .T. ) ;
#3942 = EDGE_CURVE ( 'NONE', #5044, #1974, #1669, .T. ) ;
#3943 =( NAMED_UNIT ( * ) SI_UNIT ( $, .STERADIAN. ) SOLID_ANGLE_UNIT ( ) );
#3944 = CARTESIAN_POINT ( 'NONE',  ( 1.794155980045909482, 0.000000000000000000, 4.300000000000001599 ) ) ;
#3945 = EDGE_CURVE ( 'NONE', #4799, #2669, #1566, .T. ) ;
#3946 = DIRECTION ( 'NONE',  ( 0.5150380737757185301, 1.049727191973310571E-16, 0.8571673013836900168 ) ) ;
#3947 = ORIENTED_EDGE ( 'NONE', *, *, #5301, .T. ) ;
#3948 = ORIENTED_EDGE ( 'NONE', *, *, #2254, .T. ) ;
#3949 = PLANE ( 'NONE',  #3009 ) ;
#3950 = CARTESIAN_POINT ( 'NONE',  ( 37.50000000000000711, 6.288372600415927295E-15, 75.00000000000000000 ) ) ;
#3951 = EDGE_LOOP ( 'NONE', ( #638, #1378, #3922, #3964 ) ) ;
#3952 = CARTESIAN_POINT ( 'NONE',  ( -74.99999999999998579, -15.00000000000000000, 75.00000000000000000 ) ) ;
#3953 = EDGE_CURVE ( 'NONE', #3444, #3398, #1943, .T. ) ;
#3954 = FACE_OUTER_BOUND ( 'NONE', #1658, .T. ) ;
#3955 = CARTESIAN_POINT ( 'NONE',  ( 0.000000000000000000, 0.000000000000000000, -65.00000000000000000 ) ) ;
#3956 = ORIENTED_EDGE ( 'NONE', *, *, #3090, .F. ) ;
#3957 = DIRECTION ( 'NONE',  ( 0.000000000000000000, 0.000000000000000000, 1.000000000000000000 ) ) ;
#3958 = CARTESIAN_POINT ( 'NONE',  ( 137.4999999999999716, 15.00000000000000000, -75.00000000000000000 ) ) ;
#3959 = DIRECTION ( 'NONE',  ( -0.000000000000000000, 0.000000000000000000, 1.000000000000000000 ) ) ;
#3960 = CARTESIAN_POINT ( 'NONE',  ( 37.50000000000000711, 6.288372600415927295E-15, 55.00000000000000000 ) ) ;
#3961 = DIRECTION ( 'NONE',  ( -1.000000000000000000, 0.000000000000000000, -0.000000000000000000 ) ) ;
#3962 = DIRECTION ( 'NONE',  ( -0.000000000000000000, -0.000000000000000000, -1.000000000000000000 ) ) ;
#3963 = AXIS2_PLACEMENT_3D ( 'NONE', #1947, #80, #471 ) ;
#3964 = ORIENTED_EDGE ( 'NONE', *, *, #1583, .F. ) ;
#3965 = VECTOR ( 'NONE', #4832, 1000.000000000000000 ) ;
#3966 = FACE_OUTER_BOUND ( 'NONE', #5129, .T. ) ;
#3967 =( REPRESENTATION_RELATIONSHIP ('NONE','NONE', #5609, #3184 ) REPRESENTATION_RELATIONSHIP_WITH_TRANSFORMATION ( #2591 )SHAPE_REPRESENTATION_RELATIONSHIP( ) );
#3968 = DIRECTION ( 'NONE',  ( 1.000000000000000000, 0.000000000000000000, 0.000000000000000000 ) ) ;
#3969 = VECTOR ( 'NONE', #3888, 1000.000000000000000 ) ;
#3970 = VERTEX_POINT ( 'NONE', #3565 ) ;
#3971 = FACE_BOUND ( 'NONE', #4878, .T. ) ;
#3972 = AXIS2_PLACEMENT_3D ( 'NONE', #2474, #1204, #3061 ) ;
#3973 = EDGE_CURVE ( 'NONE', #823, #2159, #5412, .T. ) ;
#3974 = CARTESIAN_POINT ( 'NONE',  ( -49.33012701892221230, 45.00000000000000000, 52.49999999999999289 ) ) ;
#3975 = EDGE_CURVE ( 'NONE', #5342, #171, #4970, .T. ) ;
#3976 = VECTOR ( 'NONE', #3472, 1000.000000000000000 ) ;
#3977 = LINE ( 'NONE', #1677, #1260 ) ;
#3979 = VERTEX_POINT ( 'NONE', #770 ) ;
#3978 = EDGE_CURVE ( 'NONE', #3934, #3708, #1738, .T. ) ;
#3980 = VERTEX_POINT ( 'NONE', #2619 ) ;
#3981 = AXIS2_PLACEMENT_3D ( 'NONE', #5900, #5940, #5420 ) ;
#3982 = VECTOR ( 'NONE', #3679, 1000.000000000000000 ) ;
#3983 = DIRECTION ( 'NONE',  ( 0.000000000000000000, 0.000000000000000000, -1.000000000000000000 ) ) ;
#3984 = SURFACE_STYLE_USAGE ( .BOTH. , #4907 ) ;
#3985 = COLOUR_RGB ( '',0.8941176470588234615, 0.8941176470588234615, 0.8941176470588234615 ) ;
#3986 = ORIENTED_EDGE ( 'NONE', *, *, #5682, .F. ) ;
#3987 = VECTOR ( 'NONE', #174, 1000.000000000000114 ) ;
#3988 = AXIS2_PLACEMENT_3D ( 'NONE', #5929, #3111, #4937 ) ;
#3989 = DIRECTION ( 'NONE',  ( -1.000000000000000000, -0.000000000000000000, -0.000000000000000000 ) ) ;
#3990 = DIRECTION ( 'NONE',  ( 0.000000000000000000, 0.000000000000000000, -1.000000000000000000 ) ) ;
#3991 = ORIENTED_EDGE ( 'NONE', *, *, #198, .T. ) ;
#3992 = FACE_OUTER_BOUND ( 'NONE', #2039, .T. ) ;
#3993 = ORIENTED_EDGE ( 'NONE', *, *, #2384, .T. ) ;
#3994 = AXIS2_PLACEMENT_3D ( 'NONE', #3137, #457, #4597 ) ;
#3995 = VECTOR ( 'NONE', #4549, 1000.000000000000000 ) ;
#3996 = ITEM_DEFINED_TRANSFORMATION ( 'NONE', 'NONE', #711,  #5080 ) ;
#3997 = AXIS2_PLACEMENT_3D ( 'NONE', #90, #66, #124 ) ;
#3998 = EDGE_CURVE ( 'NONE', #5323, #5207, #4085, .T. ) ;
#3999 = DIRECTION ( 'NONE',  ( -1.000000000000000000, 0.000000000000000000, -0.000000000000000000 ) ) ;
#4000 = CARTESIAN_POINT ( 'NONE',  ( 137.4999999999999716, 7.000000000000011546, -65.00000000000000000 ) ) ;
#4001 = DIRECTION ( 'NONE',  ( 0.000000000000000000, 1.000000000000000000, 0.000000000000000000 ) ) ;
#4002 = CARTESIAN_POINT ( 'NONE',  ( 196.6421356237309510, 0.000000000000000000, 0.000000000000000000 ) ) ;
#4003 = CARTESIAN_POINT ( 'NONE',  ( -45.00000000000001421, 50.00000000000000000, 45.00000000000000000 ) ) ;
#4004 = B_SPLINE_CURVE_WITH_KNOTS ( 'NONE', 3,
 ( #897, #2753, #421, #2263, #1989, #1535 ),
 .UNSPECIFIED., .F., .F.,
 ( 4, 2, 4 ),
 ( 0.003191392849877886309, 0.003612977948258624256, 0.004034563046639362202 ),
 .UNSPECIFIED. ) ;
#4005 = VERTEX_POINT ( 'NONE', #5005 ) ;
#4006 = CARTESIAN_POINT ( 'NONE',  ( 25.00000000000000711, -6.999999999999988454, -65.00000000000000000 ) ) ;
#4007 = ORIENTED_EDGE ( 'NONE', *, *, #3351, .T. ) ;
#4008 = CARTESIAN_POINT ( 'NONE',  ( 37.50000000000000711, 6.288372600415927295E-15, 75.00000000000000000 ) ) ;
#4009 = PRODUCT_DEFINITION_FORMATION_WITH_SPECIFIED_SOURCE ( 'ANY', '', #2234, .NOT_KNOWN. ) ;
#4010 = DIRECTION ( 'NONE',  ( 0.000000000000000000, 1.000000000000000000, 0.000000000000000000 ) ) ;
#4011 = DIRECTION ( 'NONE',  ( -0.000000000000000000, -0.000000000000000000, 1.000000000000000000 ) ) ;
#4012 = ADVANCED_FACE ( 'NONE', ( #2194 ), #5891, .F. ) ;
#4013 = VERTEX_POINT ( 'NONE', #2169 ) ;
#4014 = ORIENTED_EDGE ( 'NONE', *, *, #5643, .F. ) ;
#4015 = FACE_OUTER_BOUND ( 'NONE', #4948, .T. ) ;
#4016 = LINE ( 'NONE', #3625, #3482 ) ;
#4017 = EDGE_LOOP ( 'NONE', ( #420, #1634, #193, #4480 ) ) ;
#4018 = DIRECTION ( 'NONE',  ( 1.000000000000000000, -3.469446951953614189E-16, 0.000000000000000000 ) ) ;
#4019 = CARTESIAN_POINT ( 'NONE',  ( 137.4999999999999716, 0.000000000000000000, 0.000000000000000000 ) ) ;
#4020 = VERTEX_POINT ( 'NONE', #5328 ) ;
#4021 = CARTESIAN_POINT ( 'NONE',  ( 196.6421356237309510, 6.123233995736766282E-16, -5.000000000000000000 ) ) ;
#4022 = ADVANCED_FACE ( 'NONE', ( #3149 ), #833, .F. ) ;
#4023 = ORIENTED_EDGE ( 'NONE', *, *, #1925, .F. ) ;
#4024 = ADVANCED_FACE ( 'NONE', ( #3954 ), #5807, .F. ) ;
#4025 = LINE ( 'NONE', #3544, #2700 ) ;
#4026 = DIRECTION ( 'NONE',  ( 1.000000000000000000, 4.770489558936219510E-17, 0.000000000000000000 ) ) ;
#4027 = CARTESIAN_POINT ( 'NONE',  ( -45.00000000000001421, 0.000000000000000000, 50.00000000000000000 ) ) ;
#4028 = CARTESIAN_POINT ( 'NONE',  ( -45.00000000000001421, 40.00000000000000000, -55.00000000000000000 ) ) ;
#4029 = DIRECTION ( 'NONE',  ( -0.000000000000000000, -1.000000000000000000, -0.000000000000000000 ) ) ;
#4030 = EDGE_CURVE ( 'NONE', #4855, #2228, #2372, .T. ) ;
#4031 = ORIENTED_EDGE ( 'NONE', *, *, #4411, .T. ) ;
#4032 = DIRECTION ( 'NONE',  ( -1.000000000000000000, -0.000000000000000000, -0.000000000000000000 ) ) ;
#4033 = ORIENTED_EDGE ( 'NONE', *, *, #2005, .T. ) ;
#4034 = CARTESIAN_POINT ( 'NONE',  ( 150.0000000000000284, 15.00000000000000000, 40.00000000000000711 ) ) ;
#4035 = PRODUCT_CONTEXT ( 'NONE', #1484, 'mechanical' ) ;
#4036 = DIRECTION ( 'NONE',  ( 0.000000000000000000, 1.000000000000000000, 0.000000000000000000 ) ) ;
#4037 = PLANE ( 'NONE',  #4563 ) ;
#4038 = ORIENTED_EDGE ( 'NONE', *, *, #4509, .F. ) ;
#4039 = VERTEX_POINT ( 'NONE', #5506 ) ;
#4040 = CARTESIAN_POINT ( 'NONE',  ( 2.740000000000000213, 0.9838866223910003317, 0.5149999999999999023 ) ) ;
#4041 = ORIENTED_EDGE ( 'NONE', *, *, #5570, .F. ) ;
#4042 = CARTESIAN_POINT ( 'NONE',  ( 37.50000000000000711, 6.288372600415927295E-15, 65.00000000000000000 ) ) ;
#4043 = CARTESIAN_POINT ( 'NONE',  ( 32.00000000000001421, 6.961928339946971399E-15, 75.00000000000000000 ) ) ;
#4044 = ORIENTED_EDGE ( 'NONE', *, *, #2719, .T. ) ;
#4045 = DIRECTION ( 'NONE',  ( 0.000000000000000000, 1.000000000000000000, 1.086455722314322026E-16 ) ) ;
#4046 = ORIENTED_EDGE ( 'NONE', *, *, #4511, .T. ) ;
#4047 = ADVANCED_FACE ( 'NONE', ( #2311 ), #3207, .T. ) ;
#4048 = EDGE_CURVE ( 'NONE', #377, #111, #5733, .T. ) ;
#4049 = CARTESIAN_POINT ( 'NONE',  ( 1.299999999999999156, 2.449293598294706414E-16, 2.000000000000000000 ) ) ;
#4050 = ADVANCED_FACE ( 'NONE', ( #920 ), #1402, .T. ) ;
#4051 = DIRECTION ( 'NONE',  ( 0.000000000000000000, -1.000000000000000000, 0.000000000000000000 ) ) ;
#4052 = DIRECTION ( 'NONE',  ( 0.000000000000000000, 0.000000000000000000, 1.000000000000000000 ) ) ;
#4053 = CARTESIAN_POINT ( 'NONE',  ( -45.00000000000001421, 15.00000000000000000, 45.00000000000000000 ) ) ;
#4054 = ORIENTED_EDGE ( 'NONE', *, *, #1643, .F. ) ;
#4055 = EDGE_CURVE ( 'NONE', #2772, #4312, #3787, .T. ) ;
#4056 =( NAMED_UNIT ( * ) SI_UNIT ( $, .STERADIAN. ) SOLID_ANGLE_UNIT ( ) );
#4057 = CARTESIAN_POINT ( 'NONE',  ( -55.00000000000001421, 30.00000000000000355, 45.00000000000000000 ) ) ;
#4058 = ADVANCED_BREP_SHAPE_REPRESENTATION ( '', ( #189, #5080 ), #5845 ) ;
#4059 = AXIS2_PLACEMENT_3D ( 'NONE', #2837, #1013, #557 ) ;
#4060 = ORIENTED_EDGE ( 'NONE', *, *, #876, .T. ) ;
#4061 = CARTESIAN_POINT ( 'NONE',  ( 162.5000000000000000, -7.000000000000013323, 75.00000000000001421 ) ) ;
#4062 =( LENGTH_UNIT ( ) NAMED_UNIT ( * ) SI_UNIT ( .MILLI., .METRE. ) );
#4063 = AXIS2_PLACEMENT_3D ( 'NONE', #5614, #1855, #1006 ) ;
#4064 = FACE_OUTER_BOUND ( 'NONE', #3414, .T. ) ;
#4065 = EDGE_CURVE ( 'NONE', #782, #1576, #5063, .T. ) ;
#4066 = CARTESIAN_POINT ( 'NONE',  ( 137.4999999999999716, 6.123233995736766282E-16, 5.000000000000000000 ) ) ;
#4067 = AXIS2_PLACEMENT_3D ( 'NONE', #5265, #1555, #2984 ) ;
#4068 = VECTOR ( 'NONE', #2281, 1000.000000000000000 ) ;
#4069 = ORIENTED_EDGE ( 'NONE', *, *, #4160, .T. ) ;
#4070 = ORIENTED_EDGE ( 'NONE', *, *, #2418, .F. ) ;
#4071 = DIRECTION ( 'NONE',  ( -0.000000000000000000, 0.000000000000000000, 1.000000000000000000 ) ) ;
#4072 =( GEOMETRIC_REPRESENTATION_CONTEXT ( 3 ) GLOBAL_UNCERTAINTY_ASSIGNED_CONTEXT ( ( #3433 ) ) GLOBAL_UNIT_ASSIGNED_CONTEXT ( ( #3920, #710, #1152 ) ) REPRESENTATION_CONTEXT ( 'NONE', 'WORKASPACE' ) );
#4073 = CIRCLE ( 'NONE', #2427, 2.500000000000000000 ) ;
#4074 =( NAMED_UNIT ( * ) SI_UNIT ( $, .STERADIAN. ) SOLID_ANGLE_UNIT ( ) );
#4075 = ORIENTED_EDGE ( 'NONE', *, *, #4507, .T. ) ;
#4076 = PLANE ( 'NONE',  #2919 ) ;
#4077 = DIRECTION ( 'NONE',  ( 0.000000000000000000, 0.000000000000000000, -1.000000000000000000 ) ) ;
#4078 = CIRCLE ( 'NONE', #590, 5.000000000000000000 ) ;
#4079 = ORIENTED_EDGE ( 'NONE', *, *, #1449, .F. ) ;
#4080 = LINE ( 'NONE', #5808, #696 ) ;
#4081 = VECTOR ( 'NONE', #2076, 1000.000000000000000 ) ;
#4082 = VERTEX_POINT ( 'NONE', #76 ) ;
#4083 = DIRECTION ( 'NONE',  ( 0.000000000000000000, 0.000000000000000000, 1.000000000000000000 ) ) ;
#4084 = AXIS2_PLACEMENT_3D ( 'NONE', #1501, #238, #5303 ) ;
#4085 = CIRCLE ( 'NONE', #5351, 2.500000000000002220 ) ;
#4086 = DIRECTION ( 'NONE',  ( 1.000000000000000000, 0.000000000000000000, 0.000000000000000000 ) ) ;
#4087 = DIRECTION ( 'NONE',  ( 1.000000000000000000, -0.000000000000000000, -0.000000000000000000 ) ) ;
#4088 = CYLINDRICAL_SURFACE ( 'NONE', #5077, 7.000000000000000000 ) ;
#4089 = CARTESIAN_POINT ( 'NONE',  ( 224.9999999999999716, -7.000000000000015987, 75.00000000000000000 ) ) ;
#4090 = EDGE_LOOP ( 'NONE', ( #1186, #3375, #1581, #3193 ) ) ;
#4091 = AXIS2_PLACEMENT_3D ( 'NONE', #426, #2271, #5514 ) ;
#4092 = AXIS2_PLACEMENT_3D ( 'NONE', #4620, #3700, #5575 ) ;
#4093 = EDGE_CURVE ( 'NONE', #3220, #4439, #4570, .T. ) ;
#4094 = DIRECTION ( 'NONE',  ( 0.000000000000000000, 0.000000000000000000, 1.000000000000000000 ) ) ;
#4095 = CIRCLE ( 'NONE', #4201, 12.00000000000000000 ) ;
#4096 = AXIS2_PLACEMENT_3D ( 'NONE', #134, #940, #2795 ) ;
#4097 = ADVANCED_FACE ( 'NONE', ( #3263 ), #1280, .F. ) ;
#4098 = AXIS2_PLACEMENT_3D ( 'NONE', #4701, #2381, #84 ) ;
#4099 = EDGE_LOOP ( 'NONE', ( #2383, #3986, #5294, #3352 ) ) ;
#4100 = FACE_BOUND ( 'NONE', #3360, .T. ) ;
#4101 = PRESENTATION_LAYER_ASSIGNMENT (  '', '', ( #4298 ) ) ;
#4102 = LINE ( 'NONE', #1848, #5359 ) ;
#4103 = CARTESIAN_POINT ( 'NONE',  ( -45.00000000000001421, 0.000000000000000000, 39.99999999999999289 ) ) ;
#4104 = AXIS2_PLACEMENT_3D ( 'NONE', #1530, #3385, #177 ) ;
#4105 = ORIENTED_EDGE ( 'NONE', *, *, #1022, .T. ) ;
#4106 = EDGE_CURVE ( 'NONE', #283, #5207, #2710, .T. ) ;
#4107 = ORIENTED_EDGE ( 'NONE', *, *, #5316, .F. ) ;
#4108 = VECTOR ( 'NONE', #3279, 1000.000000000000000 ) ;
#4109 = DIRECTION ( 'NONE',  ( 1.000000000000000000, 0.000000000000000000, 0.000000000000000000 ) ) ;
#4110 = FILL_AREA_STYLE ('',( #829 ) ) ;
#4111 = EDGE_LOOP ( 'NONE', ( #4680, #5499, #5024, #5569 ) ) ;
#4112 = DIRECTION ( 'NONE',  ( -1.000000000000000000, -0.000000000000000000, -0.000000000000000000 ) ) ;
#4113 = VECTOR ( 'NONE', #5165, 1000.000000000000000 ) ;
#4114 = FACE_OUTER_BOUND ( 'NONE', #5790, .T. ) ;
#4115 = PRODUCT ( 'MAS-179', 'MAS-179', '', ( #4035 ) ) ;
#4116 = ORIENTED_EDGE ( 'NONE', *, *, #2129, .F. ) ;
#4117 = CARTESIAN_POINT ( 'NONE',  ( -74.99999999999998579, 15.00000000000000000, 75.00000000000000000 ) ) ;
#4118 = VERTEX_POINT ( 'NONE', #3714 ) ;
#4119 = CARTESIAN_POINT ( 'NONE',  ( 77.00000000000001421, 0.000000000000000000, 0.000000000000000000 ) ) ;
#4120 = CIRCLE ( 'NONE', #1640, 5.000000000000004441 ) ;
#4121 = DIRECTION ( 'NONE',  ( 1.000000000000000000, 0.000000000000000000, 0.000000000000000000 ) ) ;
#4122 = DIRECTION ( 'NONE',  ( 0.000000000000000000, 0.000000000000000000, -1.000000000000000000 ) ) ;
#4123 = CARTESIAN_POINT ( 'NONE',  ( 0.3074992278157512304, 2.196686566159293807, -2.407412430484044816E-32 ) ) ;
#4124 = AXIS2_PLACEMENT_3D ( 'NONE', #2675, #2706, #4139 ) ;
#4125 = CARTESIAN_POINT ( 'NONE',  ( 0.000000000000000000, 2.349999999999998312, -0.5150000000000000133 ) ) ;
#4126 = ORIENTED_EDGE ( 'NONE', *, *, #2953, .F. ) ;
#4127 = AXIS2_PLACEMENT_3D ( 'NONE', #3576, #398, #2240 ) ;
#4128 = CYLINDRICAL_SURFACE ( 'NONE', #4914, 7.000000000000000000 ) ;
#4129 = ORIENTED_EDGE ( 'NONE', *, *, #3104, .T. ) ;
#4130 = LINE ( 'NONE', #4034, #1763 ) ;
#4131 = CARTESIAN_POINT ( 'NONE',  ( -45.00000000000001421, 30.00000000000000355, 52.50000000000000000 ) ) ;
#4132 = EDGE_CURVE ( 'NONE', #5946, #2658, #3600, .T. ) ;
#4133 = EDGE_CURVE ( 'NONE', #4013, #51, #412, .T. ) ;
#4134 = FACE_OUTER_BOUND ( 'NONE', #2115, .T. ) ;
#4135 = VECTOR ( 'NONE', #2814, 1000.000000000000000 ) ;
#4136 = ORIENTED_EDGE ( 'NONE', *, *, #2899, .T. ) ;
#4137 = ORIENTED_EDGE ( 'NONE', *, *, #3818, .T. ) ;
#4138 = EDGE_CURVE ( 'NONE', #2197, #4461, #4381, .T. ) ;
#4139 = DIRECTION ( 'NONE',  ( 0.000000000000000000, 0.000000000000000000, -1.000000000000000000 ) ) ;
#4140 = CONTEXT_DEPENDENT_SHAPE_REPRESENTATION ( #2333, #1444 ) ;
#4141 = CARTESIAN_POINT ( 'NONE',  ( 137.4999999999999716, 7.000000000000011546, -75.00000000000000000 ) ) ;
#4142 = VERTEX_POINT ( 'NONE', #497 ) ;
#4143 = DIRECTION ( 'NONE',  ( 0.8949343913984706411, -0.4461977533473793223, 7.082407382381129037E-17 ) ) ;
#4144 = CARTESIAN_POINT ( 'NONE',  ( 67.00000000000001421, 8.572527594031473190E-16, 7.000000000000000000 ) ) ;
#4145 = ORIENTED_EDGE ( 'NONE', *, *, #333, .F. ) ;
#4146 = ORIENTED_EDGE ( 'NONE', *, *, #2000, .F. ) ;
#4147 = DIRECTION ( 'NONE',  ( 0.000000000000000000, -5.421010862427519705E-17, 1.000000000000000000 ) ) ;
#4148 = EDGE_CURVE ( 'NONE', #5213, #4738, #5117, .T. ) ;
#4149 = CARTESIAN_POINT ( 'NONE',  ( 67.00000000000000000, 0.000000000000000000, -10.49999999999999822 ) ) ;
#4150 = FACE_OUTER_BOUND ( 'NONE', #5462, .T. ) ;
#4151 = DIRECTION ( 'NONE',  ( -1.000000000000000000, 0.000000000000000000, 0.000000000000000000 ) ) ;
#4152 = PLANE ( 'NONE',  #4279 ) ;
#4153 = ORIENTED_EDGE ( 'NONE', *, *, #5640, .T. ) ;
#4154 = DIRECTION ( 'NONE',  ( 0.000000000000000000, 0.000000000000000000, 1.000000000000000000 ) ) ;
#4155 = DIRECTION ( 'NONE',  ( 1.000000000000000000, 0.000000000000000000, 0.000000000000000000 ) ) ;
#4156 = DIRECTION ( 'NONE',  ( 0.000000000000000000, 0.000000000000000000, 1.000000000000000000 ) ) ;
#4157 =( NAMED_UNIT ( * ) PLANE_ANGLE_UNIT ( ) SI_UNIT ( $, .RADIAN. ) );
#4158 = CARTESIAN_POINT ( 'NONE',  ( -45.00000000000002842, 15.00000000000000000, -49.99999999999998579 ) ) ;
#4159 = VECTOR ( 'NONE', #3766, 1000.000000000000000 ) ;
#4160 = EDGE_CURVE ( 'NONE', #3914, #2669, #2801, .T. ) ;
#4161 = ORIENTED_EDGE ( 'NONE', *, *, #537, .F. ) ;
#4162 = AXIS2_PLACEMENT_3D ( 'NONE', #821, #5495, #1331 ) ;
#4163 = AXIS2_PLACEMENT_3D ( 'NONE', #3545, #5039, #2688 ) ;
#4164 = FACE_OUTER_BOUND ( 'NONE', #2282, .T. ) ;
#4165 = CONTEXT_DEPENDENT_SHAPE_REPRESENTATION ( #3662, #1838 ) ;
#4166 = ADVANCED_FACE ( 'NONE', ( #4114 ), #4577, .T. ) ;
#4167 = AXIS2_PLACEMENT_3D ( 'NONE', #5009, #838, #2686 ) ;
#4168 = PRODUCT_DEFINITION_SHAPE ( 'NONE', 'NONE',  #5987 ) ;
#4169 = AXIS2_PLACEMENT_3D ( 'NONE', #2462, #163, #5320 ) ;
#4170 = LINE ( 'NONE', #443, #98 ) ;
#4171 = VERTEX_POINT ( 'NONE', #1829 ) ;
#4172 = ADVANCED_FACE ( 'NONE', ( #5586 ), #2833, .T. ) ;
#4173 = DIRECTION ( 'NONE',  ( -0.000000000000000000, -0.000000000000000000, 1.000000000000000000 ) ) ;
#4174 = VERTEX_POINT ( 'NONE', #1315 ) ;
#4175 = EDGE_LOOP ( 'NONE', ( #3530, #3132, #5427, #78, #2909, #1636, #2275 ) ) ;
#4176 = CIRCLE ( 'NONE', #3685, 2.500000000000002220 ) ;
#4177 = CARTESIAN_POINT ( 'NONE',  ( 162.5000000000000000, 15.00000000000000000, -75.00000000000000000 ) ) ;
#4178 = DIRECTION ( 'NONE',  ( 1.000000000000000000, -0.000000000000000000, -0.000000000000000000 ) ) ;
#4179 = CIRCLE ( 'NONE', #4167, 2.000000000000000000 ) ;
#4180 = CONICAL_SURFACE ( 'NONE', #5238, 2.500000000000002220, 1.029744260000002631 ) ;
#4181 = LINE ( 'NONE', #2866, #4667 ) ;
#4182 = CARTESIAN_POINT ( 'NONE',  ( 75.00000000000001421, 0.000000000000000000, 12.00000000000000000 ) ) ;
#4183 = FACE_OUTER_BOUND ( 'NONE', #891, .T. ) ;
#4184 = ORIENTED_EDGE ( 'NONE', *, *, #1053, .T. ) ;
#4185 = EDGE_CURVE ( 'NONE', #171, #2598, #5253, .T. ) ;
#4186 = VECTOR ( 'NONE', #4333, 1000.000000000000000 ) ;
#4187 = SHAPE_REPRESENTATION_RELATIONSHIP ( 'NONE' , 'NONE' ,  #5016, #5436 ) ;
#4188 = CIRCLE ( 'NONE', #3223, 4.750000000000000000 ) ;
#4189 = DIRECTION ( 'NONE',  ( -0.000000000000000000, -1.000000000000000000, -0.000000000000000000 ) ) ;
#4190 = CIRCLE ( 'NONE', #4287, 1.928074011315806136 ) ;
#4192 = CIRCLE ( 'NONE', #2827, 7.000000000000000000 ) ;
#4191 = LINE ( 'NONE', #271, #1946 ) ;
#4193 = ORIENTED_EDGE ( 'NONE', *, *, #3138, .F. ) ;
#4194 = TOROIDAL_SURFACE ( 'NONE', #4977, 2.700000000000000178, 0.2000000000000000111 ) ;
#4195 = FACE_OUTER_BOUND ( 'NONE', #3640, .T. ) ;
#4196 = MECHANICAL_DESIGN_GEOMETRIC_PRESENTATION_REPRESENTATION (  '', ( #4682 ), #3517 ) ;
#4197 = COLOUR_RGB ( '',0.8941176470588234615, 0.8941176470588234615, 0.8941176470588234615 ) ;
#4198 = ORIENTED_EDGE ( 'NONE', *, *, #1714, .T. ) ;
#4199 = FACE_OUTER_BOUND ( 'NONE', #3858, .T. ) ;
#4200 = CARTESIAN_POINT ( 'NONE',  ( 3.016506661494197328, 0.000000000000000000, 7.007546303702493782E-17 ) ) ;
#4201 = AXIS2_PLACEMENT_3D ( 'NONE', #2338, #5922, #1771 ) ;
#4202 = COLOUR_RGB ( '',0.8941176470588234615, 0.8941176470588234615, 0.8941176470588234615 ) ;
#4203 = DIRECTION ( 'NONE',  ( -1.000000000000000000, 0.000000000000000000, 0.000000000000000000 ) ) ;
#4204 = ORIENTED_EDGE ( 'NONE', *, *, #5738, .T. ) ;
#4205 = DIRECTION ( 'NONE',  ( 0.000000000000000000, 0.000000000000000000, 1.000000000000000000 ) ) ;
#4206 = MANIFOLD_SOLID_BREP ( 'CBORE for M5 Pan Head Screw1', #1303 ) ;
#4207 = ORIENTED_EDGE ( 'NONE', *, *, #396, .F. ) ;
#4208 = AXIS2_PLACEMENT_3D ( 'NONE', #462, #5557, #2217 ) ;
#4209 = VERTEX_POINT ( 'NONE', #1032 ) ;
#4210 = DIRECTION ( 'NONE',  ( 1.000000000000000000, -0.000000000000000000, -0.000000000000000000 ) ) ;
#4211 =( REPRESENTATION_RELATIONSHIP ('NONE','NONE', #5609, #951 ) REPRESENTATION_RELATIONSHIP_WITH_TRANSFORMATION ( #1092 )SHAPE_REPRESENTATION_RELATIONSHIP( ) );
#4212 = LINE ( 'NONE', #3244, #5220 ) ;
#4213 = FACE_OUTER_BOUND ( 'NONE', #2098, .T. ) ;
#4214 = EDGE_CURVE ( 'NONE', #3708, #3457, #992, .T. ) ;
#4215 = CARTESIAN_POINT ( 'NONE',  ( 137.4999999999999716, 15.00000000000000000, 75.00000000000001421 ) ) ;
#4216 = CARTESIAN_POINT ( 'NONE',  ( 25.00000000000000711, 1.734723475976807094E-14, 0.000000000000000000 ) ) ;
#4217 = ORIENTED_EDGE ( 'NONE', *, *, #3801, .T. ) ;
#4218 = DIRECTION ( 'NONE',  ( 1.000000000000000000, 0.000000000000000000, 0.000000000000000000 ) ) ;
#4219 = DIRECTION ( 'NONE',  ( 0.000000000000000000, 1.000000000000000000, 0.000000000000000000 ) ) ;
#4220 = EDGE_CURVE ( 'NONE', #3457, #3708, #3027, .T. ) ;
#4221 = DIRECTION ( 'NONE',  ( 0.000000000000000000, 1.000000000000000000, 0.000000000000000000 ) ) ;
#4223 = ORIENTED_EDGE ( 'NONE', *, *, #367, .F. ) ;
#4222 = PRODUCT_DEFINITION_SHAPE ( 'NONE', 'NONE',  #791 ) ;
#4224 = DIRECTION ( 'NONE',  ( 0.000000000000000000, 1.000000000000000000, 0.000000000000000000 ) ) ;
#4225 = SHAPE_REPRESENTATION ( 'piston', ( #5080 ), #3039 ) ;
#4226 = ADVANCED_FACE ( 'NONE', ( #4440 ), #3348, .T. ) ;
#4227 = VERTEX_POINT ( 'NONE', #3760 ) ;
#4228 = DIRECTION ( 'NONE',  ( -1.000000000000000000, -0.000000000000000000, -0.000000000000000000 ) ) ;
#4229 = DIRECTION ( 'NONE',  ( -0.000000000000000000, -1.000000000000000000, -0.000000000000000000 ) ) ;
#4230 = CONICAL_SURFACE ( 'NONE', #837, 0.8509999999999999787, 0.06981317007976602096 ) ;
#4231 = DIRECTION ( 'NONE',  ( 0.000000000000000000, 0.000000000000000000, 1.000000000000000000 ) ) ;
#4232 = ORIENTED_EDGE ( 'NONE', *, *, #2791, .T. ) ;
#4233 = EDGE_LOOP ( 'NONE', ( #5725, #3889, #1778, #2842 ) ) ;
#4234 = AXIS2_PLACEMENT_3D ( 'NONE', #3084, #1229, #2174 ) ;
#4235 =( NAMED_UNIT ( * ) PLANE_ANGLE_UNIT ( ) SI_UNIT ( $, .RADIAN. ) );
#4236 = DIRECTION ( 'NONE',  ( 1.000000000000000000, 0.000000000000000000, -0.000000000000000000 ) ) ;
#4237 = ORIENTED_EDGE ( 'NONE', *, *, #2346, .T. ) ;
#4238 = DIRECTION ( 'NONE',  ( 0.000000000000000000, -1.000000000000000000, -3.702006032529638986E-15 ) ) ;
#4239 = CARTESIAN_POINT ( 'NONE',  ( -45.00000000000001421, 28.00000000000000355, 52.50000000000000000 ) ) ;
#4240 = LINE ( 'NONE', #3297, #5245 ) ;
#4241 = EDGE_LOOP ( 'NONE', ( #5233, #3105 ) ) ;
#4242 = ADVANCED_FACE ( 'NONE', ( #5221 ), #138, .F. ) ;
#4243 = AXIS2_PLACEMENT_3D ( 'NONE', #4456, #1780, #296 ) ;
#4244 = SURFACE_STYLE_FILL_AREA ( #35 ) ;
#4245 = EDGE_CURVE ( 'NONE', #5520, #2883, #4388, .T. ) ;
#4246 = DIRECTION ( 'NONE',  ( -0.000000000000000000, -0.000000000000000000, -1.000000000000000000 ) ) ;
#4247 = EDGE_CURVE ( 'NONE', #4780, #3756, #2921, .T. ) ;
#4248 = CARTESIAN_POINT ( 'NONE',  ( 24.99999999999998224, 6.999999999999985789, 75.00000000000000000 ) ) ;
#4249 = EDGE_CURVE ( 'NONE', #3970, #3262, #4900, .T. ) ;
#4250 = CARTESIAN_POINT ( 'NONE',  ( 162.5000000000000000, 0.000000000000000000, 0.000000000000000000 ) ) ;
#4251 = ORIENTED_EDGE ( 'NONE', *, *, #2050, .T. ) ;
#4252 = ORIENTED_EDGE ( 'NONE', *, *, #2086, .F. ) ;
#4253 = CARTESIAN_POINT ( 'NONE',  ( 62.50000000000001421, -1.951563910473909559E-15, 71.29999999999999716 ) ) ;
#4254 = MANIFOLD_SOLID_BREP ( 'AdvancedHole4', #3534 ) ;
#4255 = ORIENTED_EDGE ( 'NONE', *, *, #656, .T. ) ;
#4256 = DIRECTION ( 'NONE',  ( 0.000000000000000000, 0.000000000000000000, -1.000000000000000000 ) ) ;
#4257 = ADVANCED_FACE ( 'NONE', ( #5463, #3163, #4991, #3971 ), #1359, .F. ) ;
#4258 = DIRECTION ( 'NONE',  ( -0.000000000000000000, -1.000000000000000000, -0.000000000000000000 ) ) ;
#4259 = ITEM_DEFINED_TRANSFORMATION ( 'NONE', 'NONE', #4890,  #5080 ) ;
#4260 = DIRECTION ( 'NONE',  ( -0.000000000000000000, -0.000000000000000000, -1.000000000000000000 ) ) ;
#4261 = AXIS2_PLACEMENT_3D ( 'NONE', #3741, #28, #3719 ) ;
#4262 = FILL_AREA_STYLE_COLOUR ( '', #797 ) ;
#4263 = ORIENTED_EDGE ( 'NONE', *, *, #5574, .T. ) ;
#4264 = ORIENTED_EDGE ( 'NONE', *, *, #5498, .F. ) ;
#4265 = COLOUR_RGB ( '',0.8941176470588234615, 0.8941176470588234615, 0.8941176470588234615 ) ;
#4266 = DIRECTION ( 'NONE',  ( 0.4461977533473793778, -2.936240938438015166E-15, 0.8949343913984707521 ) ) ;
#4267 = VERTEX_POINT ( 'NONE', #5494 ) ;
#4268 = CARTESIAN_POINT ( 'NONE',  ( 2.740000000000000213, -0.6774776749089230776, 0.5149999999999995692 ) ) ;
#4269 = CARTESIAN_POINT ( 'NONE',  ( 25.00000000000000711, -6.999999999999989342, -75.00000000000000000 ) ) ;
#4270 = PRODUCT_DEFINITION_SHAPE ( 'NONE', 'NONE',  #5972 ) ;
#4271 = CARTESIAN_POINT ( 'NONE',  ( 2.740000000000000213, -0.9838866223905674557, -0.5150000000000000133 ) ) ;
#4272 = EDGE_LOOP ( 'NONE', ( #5894, #2464 ) ) ;
#4273 = DIRECTION ( 'NONE',  ( -0.000000000000000000, -1.000000000000000000, -0.000000000000000000 ) ) ;
#4274 = AXIS2_PLACEMENT_3D ( 'NONE', #2492, #651, #2560 ) ;
#4275 = CARTESIAN_POINT ( 'NONE',  ( 24.99999999999998224, -6.999999999999985789, -75.00000000000000000 ) ) ;
#4276 = CARTESIAN_POINT ( 'NONE',  ( 0.5000000000000000000, 0.2499999999999982792, 1.911797424705720339 ) ) ;
#4277 = EDGE_CURVE ( 'NONE', #3980, #5881, #4130, .T. ) ;
#4278 = VERTEX_POINT ( 'NONE', #3669 ) ;
#4279 = AXIS2_PLACEMENT_3D ( 'NONE', #4727, #5075, #4638 ) ;
#4280 = AXIS2_PLACEMENT_3D ( 'NONE', #212, #722, #5785 ) ;
#4281 = EDGE_LOOP ( 'NONE', ( #5398, #1648, #905, #5959 ) ) ;
#4282 = FACE_OUTER_BOUND ( 'NONE', #786, .T. ) ;
#4283 = UNCERTAINTY_MEASURE_WITH_UNIT (LENGTH_MEASURE( 1.000000000000000082E-05 ), #1212, 'distance_accuracy_value', 'NONE');
#4284 = AXIS2_PLACEMENT_3D ( 'NONE', #2989, #3926, #2562 ) ;
#4285 = VECTOR ( 'NONE', #4332, 1000.000000000000000 ) ;
#4286 = ORIENTED_EDGE ( 'NONE', *, *, #2307, .F. ) ;
#4287 = AXIS2_PLACEMENT_3D ( 'NONE', #5339, #3031, #724 ) ;
#4288 = LINE ( 'NONE', #4739, #1380 ) ;
#4289 = CIRCLE ( 'NONE', #3705, 5.000000000000004441 ) ;
#4290 = PLANE ( 'NONE',  #3171 ) ;
#4291 = CARTESIAN_POINT ( 'NONE',  ( 162.5000000000000000, -6.999999999999985789, 75.00000000000001421 ) ) ;
#4292 = CIRCLE ( 'NONE', #37, 5.000000000000004441 ) ;
#4293 = EDGE_CURVE ( 'NONE', #4498, #1123, #1304, .T. ) ;
#4294 = ORIENTED_EDGE ( 'NONE', *, *, #5426, .F. ) ;
#4295 = CIRCLE ( 'NONE', #4881, 5.499999999999991118 ) ;
#4296 = VERTEX_POINT ( 'NONE', #911 ) ;
#4297 = DIRECTION ( 'NONE',  ( -1.000000000000000000, 0.000000000000000000, 0.000000000000000000 ) ) ;
#4298 = STYLED_ITEM ( 'NONE', ( #3431 ), #1882 ) ;
#4299 = DIRECTION ( 'NONE',  ( 1.000000000000000000, 0.000000000000000000, 0.000000000000000000 ) ) ;
#4300 = ORIENTED_EDGE ( 'NONE', *, *, #727, .T. ) ;
#4301 = FACE_OUTER_BOUND ( 'NONE', #4625, .T. ) ;
#4302 = CARTESIAN_POINT ( 'NONE',  ( -35.00000000000000711, 30.00000000000000355, 45.00000000000000000 ) ) ;
#4303 = PRODUCT_DEFINITION_FORMATION_WITH_SPECIFIED_SOURCE ( 'ANY', '', #1927, .NOT_KNOWN. ) ;
#4304 = CARTESIAN_POINT ( 'NONE',  ( 77.00000000000001421, 0.000000000000000000, -9.500000000000000000 ) ) ;
#4305 = ORIENTED_EDGE ( 'NONE', *, *, #3277, .T. ) ;
#4306 = SHAPE_DEFINITION_REPRESENTATION ( #4222, #1113 ) ;
#4307 = DIRECTION ( 'NONE',  ( -0.000000000000000000, -1.000000000000000000, -0.000000000000000000 ) ) ;
#4308 = CARTESIAN_POINT ( 'NONE',  ( -45.00000000000001421, 30.00000000000000355, 45.00000000000000000 ) ) ;
#4309 = CARTESIAN_POINT ( 'NONE',  ( 224.9999999999999716, -7.000000000000015987, 65.00000000000000000 ) ) ;
#4310 = DIRECTION ( 'NONE',  ( 0.000000000000000000, -1.000000000000000000, -1.652937667529658626E-16 ) ) ;
#4311 = CARTESIAN_POINT ( 'NONE',  ( 137.4999999999999716, 0.000000000000000000, 0.000000000000000000 ) ) ;
#4312 = VERTEX_POINT ( 'NONE', #5909 ) ;
#4313 = ORIENTED_EDGE ( 'NONE', *, *, #1287, .F. ) ;
#4314 = DIRECTION ( 'NONE',  ( -0.000000000000000000, -0.000000000000000000, 1.000000000000000000 ) ) ;
#4315 = EDGE_LOOP ( 'NONE', ( #273, #4952 ) ) ;
#4316 = FACE_OUTER_BOUND ( 'NONE', #619, .T. ) ;
#4317 = EDGE_CURVE ( 'NONE', #2079, #1813, #1328, .T. ) ;
#4318 = DIRECTION ( 'NONE',  ( -1.000000000000000000, -0.000000000000000000, -0.000000000000000000 ) ) ;
#4319 = ADVANCED_FACE ( 'NONE', ( #1759 ), #5020, .T. ) ;
#4320 =( REPRESENTATION_RELATIONSHIP ('NONE','NONE', #5609, #1113 ) REPRESENTATION_RELATIONSHIP_WITH_TRANSFORMATION ( #294 )SHAPE_REPRESENTATION_RELATIONSHIP( ) );
#4321 = DIRECTION ( 'NONE',  ( -1.000000000000000000, 0.000000000000000000, -0.000000000000000000 ) ) ;
#4322 = AXIS2_PLACEMENT_3D ( 'NONE', #1391, #5424, #5079 ) ;
#4324 = ORIENTED_EDGE ( 'NONE', *, *, #3978, .F. ) ;
#4323 = EDGE_CURVE ( 'NONE', #1926, #2685, #849, .T. ) ;
#4325 = EDGE_LOOP ( 'NONE', ( #508, #5594, #1026, #1236 ) ) ;
#4326 = VECTOR ( 'NONE', #4774, 1000.000000000000000 ) ;
#4327 = DIRECTION ( 'NONE',  ( -0.000000000000000000, -1.000000000000000000, -0.000000000000000000 ) ) ;
#4328 = AXIS2_PLACEMENT_3D ( 'NONE', #1785, #847, #4987 ) ;
#4329 = CARTESIAN_POINT ( 'NONE',  ( 25.00000000000000711, 7.000000000000011546, 75.00000000000000000 ) ) ;
#4330 = ORIENTED_EDGE ( 'NONE', *, *, #5574, .F. ) ;
#4331 = CARTESIAN_POINT ( 'NONE',  ( 1.424271237134740131, 0.000000000000000000, 0.000000000000000000 ) ) ;
#4332 = DIRECTION ( 'NONE',  ( -0.000000000000000000, -1.000000000000000000, -0.000000000000000000 ) ) ;
#4333 = DIRECTION ( 'NONE',  ( 0.000000000000000000, 0.000000000000000000, -1.000000000000000000 ) ) ;
#4334 = ORIENTED_EDGE ( 'NONE', *, *, #938, .F. ) ;
#4335 = DIRECTION ( 'NONE',  ( 0.000000000000000000, 0.9242245927363030855, 0.3818493186865927203 ) ) ;
#4336 = ADVANCED_FACE ( 'NONE', ( #3194 ), #2698, .T. ) ;
#4337 = DIRECTION ( 'NONE',  ( 0.000000000000000000, 0.000000000000000000, -1.000000000000000000 ) ) ;
#4338 = CIRCLE ( 'NONE', #2482, 7.000000000000000000 ) ;
#4339 = CARTESIAN_POINT ( 'NONE',  ( 40.00000000000000711, 6.288372600415927295E-15, 55.00000000000000000 ) ) ;
#4340 = CYLINDRICAL_SURFACE ( 'NONE', #3298, 2.500000000000002220 ) ;
#4341 = DIRECTION ( 'NONE',  ( 0.000000000000000000, 0.000000000000000000, 1.000000000000000000 ) ) ;
#4342 = ORIENTED_EDGE ( 'NONE', *, *, #1344, .T. ) ;
#4343 = ORIENTED_EDGE ( 'NONE', *, *, #3628, .F. ) ;
#4344 =( NAMED_UNIT ( * ) SI_UNIT ( $, .STERADIAN. ) SOLID_ANGLE_UNIT ( ) );
#4345 = CARTESIAN_POINT ( 'NONE',  ( 0.06760930072668806801, -4.837354856632045452E-15, 0.000000000000000000 ) ) ;
#4346 = UNCERTAINTY_MEASURE_WITH_UNIT (LENGTH_MEASURE( 1.000000000000000082E-05 ), #3816, 'distance_accuracy_value', 'NONE');
#4347 = ORIENTED_EDGE ( 'NONE', *, *, #3287, .F. ) ;
#4348 = SURFACE_SIDE_STYLE ('',( #2605 ) ) ;
#4349 = EDGE_CURVE ( 'NONE', #3899, #5963, #5049, .T. ) ;
#4350 = DIRECTION ( 'NONE',  ( 0.000000000000000000, -1.000000000000000000, -3.491481338843133355E-15 ) ) ;
#4351 = CARTESIAN_POINT ( 'NONE',  ( 37.50000000000000711, 6.288372600415927295E-15, 71.29999999999999716 ) ) ;
#4352 = VERTEX_POINT ( 'NONE', #878 ) ;
#4353 = EDGE_CURVE ( 'NONE', #2642, #3020, #4289, .T. ) ;
#4354 = VERTEX_POINT ( 'NONE', #1814 ) ;
#4355 = ADVANCED_FACE ( 'NONE', ( #4100, #402, #2732, #5081 ), #5883, .F. ) ;
#4356 = DIRECTION ( 'NONE',  ( 0.000000000000000000, 1.000000000000000000, 0.000000000000000000 ) ) ;
#4357 = VERTEX_POINT ( 'NONE', #434 ) ;
#4358 = DIRECTION ( 'NONE',  ( -1.000000000000000000, -0.000000000000000000, -0.000000000000000000 ) ) ;
#4359 = CARTESIAN_POINT ( 'NONE',  ( 0.5000000000000000000, -0.2499999999999997780, -2.000000000000000000 ) ) ;
#4360 = CARTESIAN_POINT ( 'NONE',  ( 8.000000000000000000, -4.896755294805453861E-15, 0.5150000000000000133 ) ) ;
#4361 = ORIENTED_EDGE ( 'NONE', *, *, #1805, .F. ) ;
#4362 = CIRCLE ( 'NONE', #2805, 1.928074011315806136 ) ;
#4363 = DIRECTION ( 'NONE',  ( 0.9989374069132286316, 0.000000000000000000, -0.04608749363411584338 ) ) ;
#4364 = CARTESIAN_POINT ( 'NONE',  ( 65.00000000000001421, -1.951563910473909559E-15, 65.00000000000000000 ) ) ;
#4365 = DIRECTION ( 'NONE',  ( 0.4999999999999987232, 0.000000000000000000, -0.8660254037844393737 ) ) ;
#4366 = CIRCLE ( 'NONE', #5906, 5.000000000000000000 ) ;
#4367 = DIRECTION ( 'NONE',  ( -0.000000000000000000, -0.000000000000000000, -1.000000000000000000 ) ) ;
#4368 = DIRECTION ( 'NONE',  ( 0.8949343913984143528, -1.557891129246500526E-15, 0.4461977533474922875 ) ) ;
#4369 = DIRECTION ( 'NONE',  ( -1.000000000000000000, 0.000000000000000000, 0.000000000000000000 ) ) ;
#4370 = EDGE_CURVE ( 'NONE', #1472, #4005, #3315, .T. ) ;
#4371 = ORIENTED_EDGE ( 'NONE', *, *, #4898, .F. ) ;
#4372 = ORIENTED_EDGE ( 'NONE', *, *, #5400, .F. ) ;
#4373 = AXIS2_PLACEMENT_3D ( 'NONE', #5872, #5513, #4122 ) ;
#4374 = LINE ( 'NONE', #3066, #3144 ) ;
#4375 = EDGE_LOOP ( 'NONE', ( #3843, #183 ) ) ;
#4376 = CIRCLE ( 'NONE', #4875, 5.000000000000004441 ) ;
#4377 = AXIS2_PLACEMENT_3D ( 'NONE', #4042, #3627, #3564 ) ;
#4378 = FILL_AREA_STYLE_COLOUR ( '', #4197 ) ;
#4379 = CARTESIAN_POINT ( 'NONE',  ( 25.00000000000000711, 1.734723475976807094E-14, 0.000000000000000000 ) ) ;
#4380 = AXIS2_PLACEMENT_3D ( 'NONE', #4304, #594, #3832 ) ;
#4381 = CIRCLE ( 'NONE', #2733, 1.037871761867652065 ) ;
#4382 = DIRECTION ( 'NONE',  ( 0.000000000000000000, 0.000000000000000000, 1.000000000000000000 ) ) ;
#4383 = CONICAL_SURFACE ( 'NONE', #4677, 0.8509999999999999787, 0.06981317007976602096 ) ;
#4384 = ORIENTED_EDGE ( 'NONE', *, *, #906, .T. ) ;
#4385 = PRESENTATION_LAYER_ASSIGNMENT (  '', '', ( #984 ) ) ;
#4386 = ORIENTED_EDGE ( 'NONE', *, *, #5615, .T. ) ;
#4387 = CARTESIAN_POINT ( 'NONE',  ( 40.00000000000000711, 6.288372600415927295E-15, 65.00000000000000000 ) ) ;
#4388 = CIRCLE ( 'NONE', #2928, 1.934182851860892116 ) ;
#4389 = CARTESIAN_POINT ( 'NONE',  ( 137.4999999999999716, 15.00000000000000000, 75.00000000000001421 ) ) ;
#4390 = VERTEX_POINT ( 'NONE', #2244 ) ;
#4391 = CARTESIAN_POINT ( 'NONE',  ( -45.00000000000001421, 28.00000000000000355, 45.00000000000000000 ) ) ;
#4392 = CARTESIAN_POINT ( 'NONE',  ( 162.5000000000000000, 15.00000000000000000, -75.00000000000000000 ) ) ;
#4393 = CARTESIAN_POINT ( 'NONE',  ( 65.00000000000001421, -1.645402210687070900E-15, -55.00000000000000000 ) ) ;
#4394 = ORIENTED_EDGE ( 'NONE', *, *, #1872, .T. ) ;
#4395 =( GEOMETRIC_REPRESENTATION_CONTEXT ( 3 ) GLOBAL_UNCERTAINTY_ASSIGNED_CONTEXT ( ( #5873 ) ) GLOBAL_UNIT_ASSIGNED_CONTEXT ( ( #2695, #846, #5942 ) ) REPRESENTATION_CONTEXT ( 'NONE', 'WORKASPACE' ) );
#4396 = APPLICATION_PROTOCOL_DEFINITION ( 'draft international standard', 'automotive_design', 1998, #4943 ) ;
#4397 = EDGE_CURVE ( 'NONE', #4780, #2259, #5521, .T. ) ;
#4398 = DIRECTION ( 'NONE',  ( 1.000000000000000000, 0.000000000000000000, -0.000000000000000000 ) ) ;
#4399 = EDGE_CURVE ( 'NONE', #2059, #3630, #4531, .T. ) ;
#4400 = LINE ( 'NONE', #5239, #2431 ) ;
#4401 = DIRECTION ( 'NONE',  ( -0.000000000000000000, -0.000000000000000000, -1.000000000000000000 ) ) ;
#4402 = CARTESIAN_POINT ( 'NONE',  ( 0.000000000000000000, 0.000000000000000000, 65.00000000000000000 ) ) ;
#4403 = CARTESIAN_POINT ( 'NONE',  ( 2.740000000000000213, 0.000000000000000000, 0.000000000000000000 ) ) ;
#4404 = DIRECTION ( 'NONE',  ( -0.000000000000000000, -0.000000000000000000, -1.000000000000000000 ) ) ;
#4405 = ORIENTED_EDGE ( 'NONE', *, *, #2527, .T. ) ;
#4406 = EDGE_CURVE ( 'NONE', #5534, #2159, #5832, .T. ) ;
#4407 = ORIENTED_EDGE ( 'NONE', *, *, #3387, .T. ) ;
#4408 =( REPRESENTATION_RELATIONSHIP ('NONE','NONE', #5609, #1113 ) REPRESENTATION_RELATIONSHIP_WITH_TRANSFORMATION ( #3996 )SHAPE_REPRESENTATION_RELATIONSHIP( ) );
#4409 = DIRECTION ( 'NONE',  ( 0.000000000000000000, 1.000000000000000000, 0.000000000000000000 ) ) ;
#4410 = PRODUCT_DEFINITION_CONTEXT ( 'detailed design', #3887, 'design' ) ;
#4411 = EDGE_CURVE ( 'NONE', #1757, #3934, #4490, .T. ) ;
#4412 = ORIENTED_EDGE ( 'NONE', *, *, #4353, .T. ) ;
#4413 = CARTESIAN_POINT ( 'NONE',  ( 25.00000000000000711, 7.000000000000011546, 65.00000000000000000 ) ) ;
#4414 = EDGE_CURVE ( 'NONE', #1155, #4905, #1959, .T. ) ;
#4415 = LINE ( 'NONE', #3619, #777 ) ;
#4416 = VERTEX_POINT ( 'NONE', #1846 ) ;
#4417 = EDGE_LOOP ( 'NONE', ( #453, #898 ) ) ;
#4418 = CIRCLE ( 'NONE', #4322, 4.556291390728477886 ) ;
#4419 = CARTESIAN_POINT ( 'NONE',  ( 3.699999999999998401, 0.000000000000000000, 4.750000000000000000 ) ) ;
#4420 = EDGE_LOOP ( 'NONE', ( #5901, #2955, #3789, #4263 ) ) ;
#4421 = FACE_OUTER_BOUND ( 'NONE', #844, .T. ) ;
#4422 = DIRECTION ( 'NONE',  ( -1.000000000000000000, 0.000000000000000000, 0.000000000000000000 ) ) ;
#4423 = DIRECTION ( 'NONE',  ( 0.000000000000000000, -0.000000000000000000, -1.000000000000000000 ) ) ;
#4424 = ORIENTED_EDGE ( 'NONE', *, *, #1383, .T. ) ;
#4425 = APPLICATION_PROTOCOL_DEFINITION ( 'draft international standard', 'automotive_design', 1998, #256 ) ;
#4426 = DIRECTION ( 'NONE',  ( -1.000000000000000000, -0.000000000000000000, -0.000000000000000000 ) ) ;
#4427 = CARTESIAN_POINT ( 'NONE',  ( 1.299999999999999156, 1.224646799147353207E-16, -1.000000000000000000 ) ) ;
#4428 = FACE_OUTER_BOUND ( 'NONE', #4448, .T. ) ;
#4429 = AXIS2_PLACEMENT_3D ( 'NONE', #5690, #4189, #2901 ) ;
#4430 = CARTESIAN_POINT ( 'NONE',  ( -45.00000000000001421, 40.00000000000000000, 45.00000000000000000 ) ) ;
#4431 = FACE_OUTER_BOUND ( 'NONE', #433, .T. ) ;
#4432 = EDGE_CURVE ( 'NONE', #3162, #3745, #4870, .T. ) ;
#4433 = ORIENTED_EDGE ( 'NONE', *, *, #1126, .T. ) ;
#4434 = EDGE_CURVE ( 'NONE', #3113, #1962, #1826, .T. ) ;
#4435 = DIRECTION ( 'NONE',  ( -0.000000000000000000, -0.000000000000000000, 1.000000000000000000 ) ) ;
#4436 =( LENGTH_UNIT ( ) NAMED_UNIT ( * ) SI_UNIT ( .MILLI., .METRE. ) );
#4437 = CYLINDRICAL_SURFACE ( 'NONE', #518, 2.500000000000002220 ) ;
#4438 = EDGE_CURVE ( 'NONE', #2390, #5222, #125, .T. ) ;
#4439 = VERTEX_POINT ( 'NONE', #8 ) ;
#4440 = FACE_OUTER_BOUND ( 'NONE', #5734, .T. ) ;
#4441 = PRESENTATION_STYLE_ASSIGNMENT (( #639 ) ) ;
#4442 = DIRECTION ( 'NONE',  ( -0.5000000000000003331, 0.000000000000000000, -0.8660254037844383745 ) ) ;
#4443 = DIRECTION ( 'NONE',  ( 0.000000000000000000, -1.000000000000000000, 0.000000000000000000 ) ) ;
#4444 = VERTEX_POINT ( 'NONE', #4706 ) ;
#4445 = ADVANCED_FACE ( 'NONE', ( #3338 ), #5187, .F. ) ;
#4446 = ORIENTED_EDGE ( 'NONE', *, *, #2902, .F. ) ;
#4447 = DIRECTION ( 'NONE',  ( 0.000000000000000000, -1.000000000000000000, 0.000000000000000000 ) ) ;
#4448 = EDGE_LOOP ( 'NONE', ( #2130, #1831, #999, #1124 ) ) ;
#4449 = CARTESIAN_POINT ( 'NONE',  ( 150.0000000000000284, 0.000000000000000000, -40.00000000000000711 ) ) ;
#4450 = CARTESIAN_POINT ( 'NONE',  ( 75.00000000000001421, 0.000000000000000000, -9.500000000000000000 ) ) ;
#4451 = ORIENTED_EDGE ( 'NONE', *, *, #3173, .F. ) ;
#4452 = CARTESIAN_POINT ( 'NONE',  ( 75.00000000000001421, -7.000000000000006217, 65.00000000000000000 ) ) ;
#4453 = ORIENTED_EDGE ( 'NONE', *, *, #938, .T. ) ;
#4454 = CONTEXT_DEPENDENT_SHAPE_REPRESENTATION ( #3164, #2421 ) ;
#4455 = PLANE ( 'NONE',  #4532 ) ;
#4456 = CARTESIAN_POINT ( 'NONE',  ( 150.0000000000000284, 0.000000000000000000, -45.00000000000000000 ) ) ;
#4457 = DIRECTION ( 'NONE',  ( 0.000000000000000000, 3.656775105596099119E-15, -1.000000000000000000 ) ) ;
#4458 = CYLINDRICAL_SURFACE ( 'NONE', #2046, 4.749999999999999112 ) ;
#4459 = LINE ( 'NONE', #2233, #4476 ) ;
#4460 = AXIS2_PLACEMENT_3D ( 'NONE', #110, #3802, #5654 ) ;
#4461 = VERTEX_POINT ( 'NONE', #2417 ) ;
#4462 =( NAMED_UNIT ( * ) PLANE_ANGLE_UNIT ( ) SI_UNIT ( $, .RADIAN. ) );
#4463 = CARTESIAN_POINT ( 'NONE',  ( 62.50000000000001421, -1.951563910473909559E-15, 65.00000000000000000 ) ) ;
#4464 = VECTOR ( 'NONE', #1551, 1000.000000000000000 ) ;
#4465 = EDGE_LOOP ( 'NONE', ( #622, #5667, #3495, #5091 ) ) ;
#4466 = SURFACE_STYLE_USAGE ( .BOTH. , #2603 ) ;
#4467 = MECHANICAL_DESIGN_GEOMETRIC_PRESENTATION_REPRESENTATION (  '', ( #4950 ), #961 ) ;
#4468 = VECTOR ( 'NONE', #1817, 1000.000000000000000 ) ;
#4469 = SURFACE_STYLE_USAGE ( .BOTH. , #4348 ) ;
#4470 = FACE_OUTER_BOUND ( 'NONE', #5617, .T. ) ;
#4471 = AXIS2_PLACEMENT_3D ( 'NONE', #5418, #5454, #2721 ) ;
#4472 = EDGE_CURVE ( 'NONE', #2678, #1861, #5256, .T. ) ;
#4473 = DIRECTION ( 'NONE',  ( 0.000000000000000000, 1.000000000000000000, 0.000000000000000000 ) ) ;
#4474 = ORIENTED_EDGE ( 'NONE', *, *, #1615, .F. ) ;
#4475 = EDGE_LOOP ( 'NONE', ( #2419, #4255, #5288, #5888, #3036, #4745 ) ) ;
#4476 = VECTOR ( 'NONE', #3123, 1000.000000000000000 ) ;
#4477 = AXIS2_PLACEMENT_3D ( 'NONE', #3868, #2498, #1167 ) ;
#4478 = DIRECTION ( 'NONE',  ( 0.000000000000000000, 0.000000000000000000, -1.000000000000000000 ) ) ;
#4479 = ADVANCED_FACE ( 'NONE', ( #5553 ), #3778, .F. ) ;
#4480 = ORIENTED_EDGE ( 'NONE', *, *, #1842, .F. ) ;
#4481 = CIRCLE ( 'NONE', #4964, 7.864440107515430434 ) ;
#4482=STYLED_ITEM('',(#6006),#4206);
#4483 = CARTESIAN_POINT ( 'NONE',  ( 137.4999999999999716, 15.00000000000000000, -65.00000000000000000 ) ) ;
#4484 = DIRECTION ( 'NONE',  ( 0.000000000000000000, 0.000000000000000000, 1.000000000000000000 ) ) ;
#4485 = VERTEX_POINT ( 'NONE', #1023 ) ;
#4486 = DIRECTION ( 'NONE',  ( -0.3090169943749412895, 1.164708318489094811E-16, -0.9510565162951555296 ) ) ;
#4487 = ORIENTED_EDGE ( 'NONE', *, *, #3104, .F. ) ;
#4488 = VECTOR ( 'NONE', #2766, 1000.000000000000000 ) ;
#4489 = VECTOR ( 'NONE', #1694, 1000.000000000000000 ) ;
#4490 = CIRCLE ( 'NONE', #4585, 1.000000000000000000 ) ;
#4491 = DIRECTION ( 'NONE',  ( 1.000000000000000000, 0.000000000000000000, 0.000000000000000000 ) ) ;
#4492 = CARTESIAN_POINT ( 'NONE',  ( -45.00000000000001421, 28.00000000000000355, 45.00000000000000000 ) ) ;
#4493 = CARTESIAN_POINT ( 'NONE',  ( 65.15000000000001990, -1.951563910473909559E-15, 75.00000000000000000 ) ) ;
#4494 = UNCERTAINTY_MEASURE_WITH_UNIT (LENGTH_MEASURE( 1.000000000000000082E-05 ), #4587, 'distance_accuracy_value', 'NONE');
#4495 = LINE ( 'NONE', #3187, #795 ) ;
#4496 =( GEOMETRIC_REPRESENTATION_CONTEXT ( 3 ) GLOBAL_UNCERTAINTY_ASSIGNED_CONTEXT ( ( #1540 ) ) GLOBAL_UNIT_ASSIGNED_CONTEXT ( ( #2550, #5767, #5348 ) ) REPRESENTATION_CONTEXT ( 'NONE', 'WORKASPACE' ) );
#4497 = LINE ( 'NONE', #1783, #112 ) ;
#4498 = VERTEX_POINT ( 'NONE', #2875 ) ;
#4499 = DIRECTION ( 'NONE',  ( 0.000000000000000000, 0.000000000000000000, -1.000000000000000000 ) ) ;
#4500 = ORIENTED_EDGE ( 'NONE', *, *, #2160, .T. ) ;
#4501 = CARTESIAN_POINT ( 'NONE',  ( 1.794155980045909482, 5.265981236333621429E-16, -4.300000000000001599 ) ) ;
#4502 = AXIS2_PLACEMENT_3D ( 'NONE', #2410, #2784, #1954 ) ;
#4503 =( NAMED_UNIT ( * ) SI_UNIT ( $, .STERADIAN. ) SOLID_ANGLE_UNIT ( ) );
#4504 = DIRECTION ( 'NONE',  ( 0.000000000000000000, -1.000000000000000000, 0.000000000000000000 ) ) ;
#4505 = LINE ( 'NONE', #1184, #875 ) ;
#4506 = ORIENTED_EDGE ( 'NONE', *, *, #3248, .T. ) ;
#4507 = EDGE_CURVE ( 'NONE', #1345, #2273, #5104, .T. ) ;
#4508 = ORIENTED_EDGE ( 'NONE', *, *, #2522, .F. ) ;
#4509 = EDGE_CURVE ( 'NONE', #5838, #3927, #5212, .T. ) ;
#4510 = PRESENTATION_STYLE_ASSIGNMENT (( #3532 ) ) ;
#4511 = EDGE_CURVE ( 'NONE', #5507, #5437, #2301, .T. ) ;
#4512 = CIRCLE ( 'NONE', #5490, 10.00000000000000178 ) ;
#4513 = ORIENTED_EDGE ( 'NONE', *, *, #1659, .F. ) ;
#4514 = EDGE_CURVE ( 'NONE', #1071, #635, #1508, .T. ) ;
#4515 = DIRECTION ( 'NONE',  ( -1.000000000000000000, -0.000000000000000000, -0.000000000000000000 ) ) ;
#4516 = ORIENTED_EDGE ( 'NONE', *, *, #4317, .T. ) ;
#4517 = CARTESIAN_POINT ( 'NONE',  ( -45.00000000000001421, 28.00000000000000355, 37.50000000000000000 ) ) ;
#4518 = VERTEX_POINT ( 'NONE', #3749 ) ;
#4519 = DIRECTION ( 'NONE',  ( 4.770489558936220126E-17, 1.000000000000000000, -0.000000000000000000 ) ) ;
#4520 = APPLICATION_CONTEXT ( 'automotive_design' ) ;
#4521 = CARTESIAN_POINT ( 'NONE',  ( 3.699999999999998401, 0.000000000000000000, 0.000000000000000000 ) ) ;
#4522 = CARTESIAN_POINT ( 'NONE',  ( 40.15000000000000568, 6.288372600415927295E-15, 75.00000000000000000 ) ) ;
#4523 = PLANE ( 'NONE',  #308 ) ;
#4524 = CONICAL_SURFACE ( 'NONE', #65, 0.8509999999999999787, 0.06981317007976602096 ) ;
#4525 = ORIENTED_EDGE ( 'NONE', *, *, #1348, .F. ) ;
#4526 = ADVANCED_FACE ( 'NONE', ( #1873 ), #3610, .F. ) ;
#4527 = FILL_AREA_STYLE ('',( #3222 ) ) ;
#4528 = DIRECTION ( 'NONE',  ( 1.007709689656716938E-16, 1.000000000000000000, 3.606821995490528048E-15 ) ) ;
#4529 = ORIENTED_EDGE ( 'NONE', *, *, #4406, .F. ) ;
#4530 = VECTOR ( 'NONE', #5195, 1000.000000000000000 ) ;
#4531 = LINE ( 'NONE', #2152, #5355 ) ;
#4532 = AXIS2_PLACEMENT_3D ( 'NONE', #3420, #1660, #3999 ) ;
#4533 = CARTESIAN_POINT ( 'NONE',  ( 0.9586399445693778443, 0.8293189044373067143, -0.5150000000000000133 ) ) ;
#4534 = CARTESIAN_POINT ( 'NONE',  ( 67.00000000000000000, 1.224646799147353207E-16, 10.49999999999999822 ) ) ;
#4535 = ORIENTED_EDGE ( 'NONE', *, *, #1242, .T. ) ;
#4536 = ORIENTED_EDGE ( 'NONE', *, *, #1866, .F. ) ;
#4537 = FACE_OUTER_BOUND ( 'NONE', #936, .T. ) ;
#4538 = ORIENTED_EDGE ( 'NONE', *, *, #5835, .T. ) ;
#4539 = CARTESIAN_POINT ( 'NONE',  ( 77.00000000000001421, 0.000000000000000000, -5.000000000000000000 ) ) ;
#4540 = DIRECTION ( 'NONE',  ( 0.000000000000000000, 0.000000000000000000, -1.000000000000000000 ) ) ;
#4541 = ADVANCED_FACE ( 'NONE', ( #455 ), #960, .T. ) ;
#4542 = ORIENTED_EDGE ( 'NONE', *, *, #198, .F. ) ;
#4543 = DIRECTION ( 'NONE',  ( 0.000000000000000000, 0.000000000000000000, 1.000000000000000000 ) ) ;
#4544 = ORIENTED_EDGE ( 'NONE', *, *, #1973, .T. ) ;
#4545 = CARTESIAN_POINT ( 'NONE',  ( 37.50000000000000711, 6.288372600415927295E-15, 55.00000000000000000 ) ) ;
#4546 = ADVANCED_FACE ( 'NONE', ( #3253 ), #38, .T. ) ;
#4547 = PLANE ( 'NONE',  #5040 ) ;
#4548 = CARTESIAN_POINT ( 'NONE',  ( 0.3226060873438262311, 0.5150000000000077849, -2.189154565102684025 ) ) ;
#4549 = DIRECTION ( 'NONE',  ( 1.000000000000000000, -2.312964634635742895E-17, 0.000000000000000000 ) ) ;
#4550 = CARTESIAN_POINT ( 'NONE',  ( 3.900000000000000799, 0.000000000000000000, 2.700000000000000178 ) ) ;
#4551 = EDGE_LOOP ( 'NONE', ( #2517, #2309, #709, #5776 ) ) ;
#4552 = PRODUCT_DEFINITION_SHAPE ( 'NONE', 'NONE',  #4803 ) ;
#4553 = DIRECTION ( 'NONE',  ( -1.000000000000000000, -0.000000000000000000, -0.000000000000000000 ) ) ;
#4554 = AXIS2_PLACEMENT_3D ( 'NONE', #54, #5590, #4236 ) ;
#4555 = EDGE_CURVE ( 'NONE', #2775, #4082, #4191, .T. ) ;
#4556 = ORIENTED_EDGE ( 'NONE', *, *, #3750, .F. ) ;
#4557 = VECTOR ( 'NONE', #5465, 1000.000000000000000 ) ;
#4558 = CARTESIAN_POINT ( 'NONE',  ( -45.00000000000001421, 0.000000000000000000, 45.00000000000000000 ) ) ;
#4559 = SURFACE_SIDE_STYLE ('',( #1727 ) ) ;
#4560 = AXIS2_PLACEMENT_3D ( 'NONE', #3822, #5196, #4833 ) ;
#4561 = CARTESIAN_POINT ( 'NONE',  ( 0.06760930072668842883, -0.5149999999999961275, -0.9010842325122929708 ) ) ;
#4562 = LINE ( 'NONE', #89, #3006 ) ;
#4563 = AXIS2_PLACEMENT_3D ( 'NONE', #5886, #2581, #3583 ) ;
#4564 = ORIENTED_EDGE ( 'NONE', *, *, #4133, .F. ) ;
#4565 = ORIENTED_EDGE ( 'NONE', *, *, #1646, .T. ) ;
#4566 = CARTESIAN_POINT ( 'NONE',  ( 8.000000000000000000, -4.837354856632045452E-15, 0.000000000000000000 ) ) ;
#4567 = DIRECTION ( 'NONE',  ( 1.000000000000000000, 0.000000000000000000, 0.000000000000000000 ) ) ;
#4568 = EDGE_LOOP ( 'NONE', ( #3074, #1211 ) ) ;
#4569 = DIRECTION ( 'NONE',  ( -1.000000000000000000, -0.000000000000000000, -0.000000000000000000 ) ) ;
#4570 = LINE ( 'NONE', #4658, #5627 ) ;
#4571 = CIRCLE ( 'NONE', #2542, 5.499999999999991118 ) ;
#4572 = ORIENTED_EDGE ( 'NONE', *, *, #4220, .F. ) ;
#4573 = DIRECTION ( 'NONE',  ( -1.000000000000000000, -0.000000000000000000, -0.000000000000000000 ) ) ;
#4574 = AXIS2_PLACEMENT_3D ( 'NONE', #5890, #4936, #1737 ) ;
#4575 = ORIENTED_EDGE ( 'NONE', *, *, #4353, .F. ) ;
#4576 = SURFACE_SIDE_STYLE ('',( #5536 ) ) ;
#4577 = TOROIDAL_SURFACE ( 'NONE', #3701, 4.300000000000001599, 0.4499999999999985678 ) ;
#4578 = PLANE ( 'NONE',  #5802 ) ;
#4579 = CARTESIAN_POINT ( 'NONE',  ( 0.5000000000000000000, -0.2500000000000000000, 1.911797424705720116 ) ) ;
#4580 = PLANE ( 'NONE',  #4091 ) ;
#4581 = PRODUCT_RELATED_PRODUCT_CATEGORY ( 'part', '', ( #4847 ) ) ;
#4582 = DIRECTION ( 'NONE',  ( 0.000000000000000000, 5.421010862427519705E-17, -1.000000000000000000 ) ) ;
#4583 = ORIENTED_EDGE ( 'NONE', *, *, #971, .F. ) ;
#4584 = CONICAL_SURFACE ( 'NONE', #3025, 0.8509999999999999787, 0.06981317007976602096 ) ;
#4585 = AXIS2_PLACEMENT_3D ( 'NONE', #4678, #1417, #2389 ) ;
#4586 = EDGE_CURVE ( 'NONE', #1041, #5450, #3873, .T. ) ;
#4587 =( LENGTH_UNIT ( ) NAMED_UNIT ( * ) SI_UNIT ( .MILLI., .METRE. ) );
#4588 = ADVANCED_FACE ( 'NONE', ( #2971 ), #210, .T. ) ;
#4589 = CARTESIAN_POINT ( 'NONE',  ( 0.9586399445693646326, 0.8293189044373081575, 0.5149999999999996803 ) ) ;
#4590 = AXIS2_PLACEMENT_3D ( 'NONE', #4566, #1821, #4109 ) ;
#4591 =( GEOMETRIC_REPRESENTATION_CONTEXT ( 3 ) GLOBAL_UNCERTAINTY_ASSIGNED_CONTEXT ( ( #221 ) ) GLOBAL_UNIT_ASSIGNED_CONTEXT ( ( #1761, #4157, #2246 ) ) REPRESENTATION_CONTEXT ( 'NONE', 'WORKASPACE' ) );
#4592 = ORIENTED_EDGE ( 'NONE', *, *, #4370, .T. ) ;
#4593 = EDGE_CURVE ( 'NONE', #5855, #3531, #3454, .T. ) ;
#4594 = DIRECTION ( 'NONE',  ( 0.000000000000000000, 0.000000000000000000, 1.000000000000000000 ) ) ;
#4595 = STYLED_ITEM ( 'NONE', ( #5248 ), #4722 ) ;
#4596 =( LENGTH_UNIT ( ) NAMED_UNIT ( * ) SI_UNIT ( .MILLI., .METRE. ) );
#4597 = DIRECTION ( 'NONE',  ( 1.000000000000000000, 0.000000000000000000, 0.000000000000000000 ) ) ;
#4598 = DIRECTION ( 'NONE',  ( -0.000000000000000000, -1.000000000000000000, -0.000000000000000000 ) ) ;
#4599 = PRODUCT_DEFINITION_FORMATION_WITH_SPECIFIED_SOURCE ( 'ANY', '', #4847, .NOT_KNOWN. ) ;
#4600 = VERTEX_POINT ( 'NONE', #2055 ) ;
#4601 = ORIENTED_EDGE ( 'NONE', *, *, #3660, .F. ) ;
#4602 = EDGE_CURVE ( 'NONE', #5963, #1325, #4571, .T. ) ;
#4603 = DIRECTION ( 'NONE',  ( 0.000000000000000000, 1.000000000000000000, 0.000000000000000000 ) ) ;
#4604 = CONTEXT_DEPENDENT_SHAPE_REPRESENTATION ( #3275, #3346 ) ;
#4605 = APPLICATION_CONTEXT ( 'automotive_design' ) ;
#4606 = CARTESIAN_POINT ( 'NONE',  ( 135.4999999999999716, 6.123233995736766282E-16, -5.000000000000000000 ) ) ;
#4607 = ORIENTED_EDGE ( 'NONE', *, *, #4432, .T. ) ;
#4608 = CARTESIAN_POINT ( 'NONE',  ( -45.00000000000001421, 30.00000000000000355, 39.99999999999999289 ) ) ;
#4609 = CARTESIAN_POINT ( 'NONE',  ( 65.00000000000001421, -1.645402210687070900E-15, -55.00000000000000000 ) ) ;
#4610 = ORIENTED_EDGE ( 'NONE', *, *, #3013, .T. ) ;
#4611 = ORIENTED_EDGE ( 'NONE', *, *, #4414, .T. ) ;
#4612 = FACE_BOUND ( 'NONE', #3176, .T. ) ;
#4613 = CARTESIAN_POINT ( 'NONE',  ( -9.262305278225771052E-15, -0.2499999999999999445, 1.454152683131084256 ) ) ;
#4614 = DIRECTION ( 'NONE',  ( 0.000000000000000000, 0.000000000000000000, -1.000000000000000000 ) ) ;
#4615 = DIRECTION ( 'NONE',  ( 0.000000000000000000, -1.000000000000000000, 0.000000000000000000 ) ) ;
#4616 = ORIENTED_EDGE ( 'NONE', *, *, #3169, .T. ) ;
#4617 = CARTESIAN_POINT ( 'NONE',  ( 0.000000000000000000, 0.000000000000000000, 0.000000000000000000 ) ) ;
#4618 = DIRECTION ( 'NONE',  ( 1.000000000000000000, -0.000000000000000000, -0.000000000000000000 ) ) ;
#4619 = ADVANCED_FACE ( 'NONE', ( #4431 ), #2571, .F. ) ;
#4620 = CARTESIAN_POINT ( 'NONE',  ( 62.50000000000001421, -1.951563910473909559E-15, -55.00000000000000000 ) ) ;
#4621 = EDGE_CURVE ( 'NONE', #4267, #4498, #5758, .T. ) ;
#4622 = SHAPE_REPRESENTATION_RELATIONSHIP ( 'NONE' , 'NONE' ,  #3184, #4787 ) ;
#4623 = FACE_OUTER_BOUND ( 'NONE', #3621, .T. ) ;
#4624 = ADVANCED_FACE ( 'NONE', ( #5340 ), #3392, .F. ) ;
#4625 = EDGE_LOOP ( 'NONE', ( #1090, #5116 ) ) ;
#4626 = PLANE ( 'NONE',  #4208 ) ;
#4627 = CONTEXT_DEPENDENT_SHAPE_REPRESENTATION ( #2530, #634 ) ;
#4628 = PRESENTATION_STYLE_ASSIGNMENT (( #48 ) ) ;
#4629 = EDGE_LOOP ( 'NONE', ( #5867, #5119, #4904, #1519 ) ) ;
#4630 = EDGE_CURVE ( 'NONE', #2264, #1983, #2112, .T. ) ;
#4631 = CARTESIAN_POINT ( 'NONE',  ( 196.6421356237309510, 0.000000000000000000, 0.000000000000000000 ) ) ;
#4632 = ORIENTED_EDGE ( 'NONE', *, *, #2307, .T. ) ;
#4633 = EDGE_LOOP ( 'NONE', ( #2113, #4535, #4184, #4695, #4343, #167, #321, #3485, #4161, #206, #1884, #5715, #1952 ) ) ;
#4634 = CARTESIAN_POINT ( 'NONE',  ( -35.00000000000000711, 30.00000000000000355, -45.00000000000000000 ) ) ;
#4635 = DIRECTION ( 'NONE',  ( -0.000000000000000000, -0.000000000000000000, 1.000000000000000000 ) ) ;
#4636 = DIRECTION ( 'NONE',  ( 0.000000000000000000, 0.000000000000000000, 1.000000000000000000 ) ) ;
#4637 = FACE_OUTER_BOUND ( 'NONE', #1132, .T. ) ;
#4638 = DIRECTION ( 'NONE',  ( -1.000000000000000000, 3.469446951953614189E-16, 0.000000000000000000 ) ) ;
#4639 = ORIENTED_EDGE ( 'NONE', *, *, #640, .F. ) ;
#4640 = CARTESIAN_POINT ( 'NONE',  ( 192.8782460975600941, 0.000000000000000000, -2.026120524630508513 ) ) ;
#4641 = DIRECTION ( 'NONE',  ( 0.000000000000000000, 1.000000000000000000, 0.000000000000000000 ) ) ;
#4642 = DIRECTION ( 'NONE',  ( 1.000000000000000000, -2.312964634635742895E-17, 0.000000000000000000 ) ) ;
#4643 = EDGE_LOOP ( 'NONE', ( #1463, #166, #3947, #326 ) ) ;
#4644 =( NAMED_UNIT ( * ) PLANE_ANGLE_UNIT ( ) SI_UNIT ( $, .RADIAN. ) );
#4645 = CARTESIAN_POINT ( 'NONE',  ( 65.00000000000001421, -1.951563910473909559E-15, 55.00000000000000000 ) ) ;
#4646 = AXIS2_PLACEMENT_3D ( 'NONE', #2006, #2929, #2892 ) ;
#4647 = MECHANICAL_DESIGN_GEOMETRIC_PRESENTATION_REPRESENTATION (  '', ( #394 ), #2027 ) ;
#4648 = ORIENTED_EDGE ( 'NONE', *, *, #2384, .F. ) ;
#4649 = B_SPLINE_CURVE_WITH_KNOTS ( 'NONE', 3,
 ( #3903, #5755, #2051, #1533 ),
 .UNSPECIFIED., .F., .F.,
 ( 4, 4 ),
 ( 0.001586480563516616538, 0.004268227385920363680 ),
 .UNSPECIFIED. ) ;
#4650 = AXIS2_PLACEMENT_3D ( 'NONE', #4901, #4036, #1183 ) ;
#4651 = CYLINDRICAL_SURFACE ( 'NONE', #3230, 2.649999999999999467 ) ;
#4652 = CARTESIAN_POINT ( 'NONE',  ( 75.00000000000001421, 6.999999999999993783, -65.00000000000000000 ) ) ;
#4653 = EDGE_CURVE ( 'NONE', #2273, #4783, #1111, .T. ) ;
#4654 = AXIS2_PLACEMENT_3D ( 'NONE', #1431, #423, #1379 ) ;
#4655 = AXIS2_PLACEMENT_3D ( 'NONE', #213, #3422, #269 ) ;
#4656 = FILL_AREA_STYLE ('',( #2340 ) ) ;
#4657 = EDGE_LOOP ( 'NONE', ( #2463, #2089, #1096, #1596 ) ) ;
#4658 = CARTESIAN_POINT ( 'NONE',  ( 0.000000000000000000, -2.349999999999999201, -0.5150000000000000133 ) ) ;
#4659 = ORIENTED_EDGE ( 'NONE', *, *, #1805, .T. ) ;
#4660=STYLED_ITEM('',(#6027),#216);
#4661 = EDGE_LOOP ( 'NONE', ( #2572, #990, #1171, #3168 ) ) ;
#4662 = VECTOR ( 'NONE', #3663, 1000.000000000000000 ) ;
#4663 = CARTESIAN_POINT ( 'NONE',  ( 24.99999999999998224, 6.999999999999985789, 75.00000000000000000 ) ) ;
#4664 = EDGE_CURVE ( 'NONE', #5207, #5323, #688, .T. ) ;
#4665 = LINE ( 'NONE', #2863, #5896 ) ;
#4666 = AXIS2_PLACEMENT_3D ( 'NONE', #4216, #2407, #59 ) ;
#4667 = VECTOR ( 'NONE', #558, 1000.000000000000114 ) ;
#4668 = DIRECTION ( 'NONE',  ( 0.000000000000000000, 0.000000000000000000, 1.000000000000000000 ) ) ;
#4669 = DIRECTION ( 'NONE',  ( -1.000000000000000000, -0.000000000000000000, -0.000000000000000000 ) ) ;
#4670 = CARTESIAN_POINT ( 'NONE',  ( 65.00000000000001421, -1.645402210687070900E-15, -65.00000000000000000 ) ) ;
#4671 = ORIENTED_EDGE ( 'NONE', *, *, #4214, .T. ) ;
#4672 = CIRCLE ( 'NONE', #2242, 5.000000000000000000 ) ;
#4673 = PRESENTATION_STYLE_ASSIGNMENT (( #1504 ) ) ;
#4674 = AXIS2_PLACEMENT_3D ( 'NONE', #681, #5271, #4815 ) ;
#4675 = EDGE_CURVE ( 'NONE', #2126, #3262, #4376, .T. ) ;
#4676 = FACE_OUTER_BOUND ( 'NONE', #1509, .T. ) ;
#4677 = AXIS2_PLACEMENT_3D ( 'NONE', #4403, #4759, #3932 ) ;
#4679 = VECTOR ( 'NONE', #4515, 1000.000000000000000 ) ;
#4678 = CARTESIAN_POINT ( 'NONE',  ( 9.300000000000002487, 0.000000000000000000, 0.000000000000000000 ) ) ;
#4680 = ORIENTED_EDGE ( 'NONE', *, *, #1126, .F. ) ;
#4681 = CARTESIAN_POINT ( 'NONE',  ( 135.4999999999999716, 0.000000000000000000, 0.000000000000000000 ) ) ;
#4682 = STYLED_ITEM ( 'NONE', ( #2765 ), #4787 ) ;
#4683 = AXIS2_PLACEMENT_3D ( 'NONE', #2184, #5428, #5403 ) ;
#4684 =( GEOMETRIC_REPRESENTATION_CONTEXT ( 3 ) GLOBAL_UNCERTAINTY_ASSIGNED_CONTEXT ( ( #3087 ) ) GLOBAL_UNIT_ASSIGNED_CONTEXT ( ( #430, #817, #2147 ) ) REPRESENTATION_CONTEXT ( 'NONE', 'WORKASPACE' ) );
#4685 = ORIENTED_EDGE ( 'NONE', *, *, #3318, .T. ) ;
#4686 = CARTESIAN_POINT ( 'NONE',  ( -49.33012701892221230, 45.00000000000000000, 52.49999999999999289 ) ) ;
#4687 = CYLINDRICAL_SURFACE ( 'NONE', #1611, 1.000000000000000000 ) ;
#4688 = AXIS2_PLACEMENT_3D ( 'NONE', #4818, #5276, #2965 ) ;
#4689 = CARTESIAN_POINT ( 'NONE',  ( 0.3226060873438244547, -2.189154565102685801, 0.5149999999999992362 ) ) ;
#4690 = DIRECTION ( 'NONE',  ( 0.000000000000000000, 1.000000000000000000, 0.000000000000000000 ) ) ;
#4691 = ADVANCED_FACE ( 'NONE', ( #1170 ), #4794, .T. ) ;
#4692 = ORIENTED_EDGE ( 'NONE', *, *, #2978, .T. ) ;
#4693 = ADVANCED_FACE ( 'NONE', ( #2941 ), #5371, .F. ) ;
#4694 = EDGE_CURVE ( 'NONE', #5475, #3671, #4760, .T. ) ;
#4695 = ORIENTED_EDGE ( 'NONE', *, *, #5133, .T. ) ;
#4696 = CARTESIAN_POINT ( 'NONE',  ( -45.00000000000001421, 28.00000000000000355, 39.99999999999999289 ) ) ;
#4697 = EDGE_CURVE ( 'NONE', #5459, #626, #4078, .T. ) ;
#4698 = LINE ( 'NONE', #1834, #5701 ) ;
#4699 = DIRECTION ( 'NONE',  ( 0.000000000000000000, 0.000000000000000000, -1.000000000000000000 ) ) ;
#4700 = CARTESIAN_POINT ( 'NONE',  ( -45.00000000000001421, 50.00000000000000000, 39.99999999999999289 ) ) ;
#4701 = CARTESIAN_POINT ( 'NONE',  ( 224.9999999999999716, 6.999999999999985789, 75.00000000000000000 ) ) ;
#4702 = ORIENTED_EDGE ( 'NONE', *, *, #4953, .T. ) ;
#4703 = DIRECTION ( 'NONE',  ( 0.000000000000000000, 0.000000000000000000, 1.000000000000000000 ) ) ;
#4704 = CARTESIAN_POINT ( 'NONE',  ( 0.06760930072668894231, -0.9010842325122859764, 0.5149999999999992362 ) ) ;
#4705 = CARTESIAN_POINT ( 'NONE',  ( 77.00000000000001421, 0.000000000000000000, 0.000000000000000000 ) ) ;
#4706 = CARTESIAN_POINT ( 'NONE',  ( -45.00000000000002842, 0.000000000000000000, -39.99999999999997868 ) ) ;
#4707 = ADVANCED_FACE ( 'NONE', ( #632 ), #215, .F. ) ;
#4708 = ORIENTED_EDGE ( 'NONE', *, *, #2529, .T. ) ;
#4710 = ORIENTED_EDGE ( 'NONE', *, *, #3614, .T. ) ;
#4709 = PRODUCT_DEFINITION_SHAPE ( 'NONE', 'NONE',  #5991 ) ;
#4711 = DIRECTION ( 'NONE',  ( 0.000000000000000000, 0.000000000000000000, 1.000000000000000000 ) ) ;
#4712 = APPLICATION_CONTEXT ( 'automotive_design' ) ;
#4713 = ORIENTED_EDGE ( 'NONE', *, *, #907, .F. ) ;
#4714 = LINE ( 'NONE', #2459, #3892 ) ;
#4715 = DIRECTION ( 'NONE',  ( 0.5150380737757185301, 1.049727191973310571E-16, 0.8571673013836900168 ) ) ;
#4716 = AXIS2_PLACEMENT_3D ( 'NONE', #1030, #521, #2369 ) ;
#4717 = CARTESIAN_POINT ( 'NONE',  ( 75.00000000000001421, -15.00000000000000355, 75.00000000000000000 ) ) ;
#4718 = DIRECTION ( 'NONE',  ( 0.000000000000000000, 0.000000000000000000, 1.000000000000000000 ) ) ;
#4719 = ORIENTED_EDGE ( 'NONE', *, *, #1615, .T. ) ;
#4720 = ORIENTED_EDGE ( 'NONE', *, *, #1715, .F. ) ;
#4721 = PRESENTATION_STYLE_ASSIGNMENT (( #1976 ) ) ;
#4722 = ADVANCED_BREP_SHAPE_REPRESENTATION ( '', ( #196, #5080 ), #2647 ) ;
#4723 = FACE_OUTER_BOUND ( 'NONE', #2576, .T. ) ;
#4724 = EDGE_CURVE ( 'NONE', #3012, #199, #2252, .T. ) ;
#4725 = DIRECTION ( 'NONE',  ( 1.000000000000000000, 0.000000000000000000, 0.000000000000000000 ) ) ;
#4726 = DIRECTION ( 'NONE',  ( 1.000000000000000000, 0.000000000000000000, 0.000000000000000000 ) ) ;
#4727 = CARTESIAN_POINT ( 'NONE',  ( 25.00000000000000711, 7.000000000000011546, -65.00000000000000000 ) ) ;
#4728 = ORIENTED_EDGE ( 'NONE', *, *, #1242, .F. ) ;
#4729 = ADVANCED_FACE ( 'NONE', ( #843 ), #4523, .T. ) ;
#4730 = DIRECTION ( 'NONE',  ( 0.000000000000000000, 0.000000000000000000, 1.000000000000000000 ) ) ;
#4731 = PLANE ( 'NONE',  #1613 ) ;
#4732 = CARTESIAN_POINT ( 'NONE',  ( 1.424271237134740131, 4.556291390728479662, 0.000000000000000000 ) ) ;
#4733 = CARTESIAN_POINT ( 'NONE',  ( -55.00000000000001421, 40.00000000000000000, 45.00000000000000000 ) ) ;
#4734 = ORIENTED_EDGE ( 'NONE', *, *, #5517, .F. ) ;
#4735 = ORIENTED_EDGE ( 'NONE', *, *, #4055, .F. ) ;
#4736 = PLANE ( 'NONE',  #5735 ) ;
#4737 = EDGE_CURVE ( 'NONE', #140, #2788, #3305, .T. ) ;
#4738 = VERTEX_POINT ( 'NONE', #1810 ) ;
#4739 = CARTESIAN_POINT ( 'NONE',  ( -55.00000000000001421, 40.00000000000000000, 45.00000000000000000 ) ) ;
#4740 = CARTESIAN_POINT ( 'NONE',  ( 8.000000000000000000, 0.5150000000000000133, 1.798112889504231112E-15 ) ) ;
#4741 = CARTESIAN_POINT ( 'NONE',  ( 62.50000000000001421, -1.951563910473909559E-15, 55.00000000000000000 ) ) ;
#4742 = CIRCLE ( 'NONE', #3963, 4.999999999999990230 ) ;
#4743 = DIRECTION ( 'NONE',  ( -1.000000000000000000, -0.000000000000000000, -0.000000000000000000 ) ) ;
#4744 = ORIENTED_EDGE ( 'NONE', *, *, #1174, .F. ) ;
#4745 = ORIENTED_EDGE ( 'NONE', *, *, #642, .T. ) ;
#4746 = CARTESIAN_POINT ( 'NONE',  ( 1.424271237134740131, 0.000000000000000000, 4.556291390728477886 ) ) ;
#4747 = AXIS2_PLACEMENT_3D ( 'NONE', #103, #1939, #1587 ) ;
#4748 = PLANE ( 'NONE',  #2018 ) ;
#4749 = ORIENTED_EDGE ( 'NONE', *, *, #4030, .F. ) ;
#4750 = DIRECTION ( 'NONE',  ( -1.000000000000000000, -0.000000000000000000, -0.000000000000000000 ) ) ;
#4751 = CYLINDRICAL_SURFACE ( 'NONE', #3886, 2.649999999999999467 ) ;
#4752 = AXIS2_PLACEMENT_3D ( 'NONE', #1804, #5933, #5037 ) ;
#4753 = LINE ( 'NONE', #4883, #411 ) ;
#4754 = CIRCLE ( 'NONE', #195, 5.000000000000000000 ) ;
#4755 = VERTEX_POINT ( 'NONE', #2143 ) ;
#4756 = SHAPE_DEFINITION_REPRESENTATION ( #1701, #3254 ) ;
#4757 = CARTESIAN_POINT ( 'NONE',  ( -45.00000000000001421, 40.00000000000000000, 45.00000000000000000 ) ) ;
#4758 = LINE ( 'NONE', #2702, #1845 ) ;
#4759 = DIRECTION ( 'NONE',  ( -1.000000000000000000, -0.000000000000000000, -0.000000000000000000 ) ) ;
#4760 = LINE ( 'NONE', #3841, #5914 ) ;
#4761 = ADVANCED_FACE ( 'NONE', ( #815 ), #1749, .F. ) ;
#4762 = ORIENTED_EDGE ( 'NONE', *, *, #106, .T. ) ;
#4763 = VECTOR ( 'NONE', #2297, 1000.000000000000000 ) ;
#4764 = AXIS2_PLACEMENT_3D ( 'NONE', #5062, #894, #2750 ) ;
#4765 = EDGE_CURVE ( 'NONE', #1699, #3406, #1752, .T. ) ;
#4766 = ORIENTED_EDGE ( 'NONE', *, *, #3318, .F. ) ;
#4767 = SURFACE_STYLE_USAGE ( .BOTH. , #4993 ) ;
#4768 = FACE_OUTER_BOUND ( 'NONE', #376, .T. ) ;
#4769 = CIRCLE ( 'NONE', #3699, 5.000000000000000000 ) ;
#4770 = ADVANCED_FACE ( 'NONE', ( #1695, #2597, #870 ), #3604, .F. ) ;
#4771 = AXIS2_PLACEMENT_3D ( 'NONE', #1885, #466, #1800 ) ;
#4772 = ORIENTED_EDGE ( 'NONE', *, *, #55, .F. ) ;
#4773 = LINE ( 'NONE', #4686, #900 ) ;
#4774 = DIRECTION ( 'NONE',  ( 1.000000000000000000, -4.770489558936219510E-17, 0.000000000000000000 ) ) ;
#4775 = DIRECTION ( 'NONE',  ( -0.000000000000000000, -0.000000000000000000, 1.000000000000000000 ) ) ;
#4776 =( GEOMETRIC_REPRESENTATION_CONTEXT ( 3 ) GLOBAL_UNCERTAINTY_ASSIGNED_CONTEXT ( ( #5670 ) ) GLOBAL_UNIT_ASSIGNED_CONTEXT ( ( #4596, #2185, #3195 ) ) REPRESENTATION_CONTEXT ( 'NONE', 'WORKASPACE' ) );
#4777 = FILL_AREA_STYLE ('',( #4262 ) ) ;
#4778 = ORIENTED_EDGE ( 'NONE', *, *, #4923, .T. ) ;
#4779 = EDGE_CURVE ( 'NONE', #5285, #2744, #5458, .T. ) ;
#4780 = VERTEX_POINT ( 'NONE', #5014 ) ;
#4781 = FILL_AREA_STYLE ('',( #5743 ) ) ;
#4782 = CYLINDRICAL_SURFACE ( 'NONE', #5704, 2.500000000000002220 ) ;
#4783 = VERTEX_POINT ( 'NONE', #5488 ) ;
#4784 = PLANE ( 'NONE',  #1452 ) ;
#4785 = CARTESIAN_POINT ( 'NONE',  ( 25.00000000000000711, 7.000000000000011546, -65.00000000000000000 ) ) ;
#4786 = DIRECTION ( 'NONE',  ( -0.000000000000000000, -1.000000000000000000, -0.000000000000000000 ) ) ;
#4787 = ADVANCED_BREP_SHAPE_REPRESENTATION ( '', ( #2209, #5080 ), #4591 ) ;
#4788 = ORIENTED_EDGE ( 'NONE', *, *, #2604, .T. ) ;
#4789 = DIRECTION ( 'NONE',  ( 1.000000000000000000, 0.000000000000000000, 0.000000000000000000 ) ) ;
#4790 = PLANE ( 'NONE',  #2676 ) ;
#4791 = PLANE ( 'NONE',  #789 ) ;
#4792 = CARTESIAN_POINT ( 'NONE',  ( 1.794155980045911036, 0.000000000000000000, 0.000000000000000000 ) ) ;
#4793 = CARTESIAN_POINT ( 'NONE',  ( 25.00000000000000711, -6.999999999999988454, 65.00000000000000000 ) ) ;
#4794 = PLANE ( 'NONE',  #2918 ) ;
#4795 = EDGE_LOOP ( 'NONE', ( #3991, #1060, #2889, #2190 ) ) ;
#4796 = ORIENTED_EDGE ( 'NONE', *, *, #5072, .T. ) ;
#4797 = PLANE ( 'NONE',  #5649 ) ;
#4798 = PRODUCT ( 'pan head cross recess screw_iso_ISO 7045 - M5 x 16 - Z - 16N', 'pan head cross recess screw_iso_ISO 7045 - M5 x 16 - Z - 16N', '', ( #1106 ) ) ;
#4799 = VERTEX_POINT ( 'NONE', #5970 ) ;
#4800 = EDGE_CURVE ( 'NONE', #674, #1123, #4459, .T. ) ;
#4801 = ADVANCED_FACE ( 'NONE', ( #1299 ), #2692, .F. ) ;
#4802 =( LENGTH_UNIT ( ) NAMED_UNIT ( * ) SI_UNIT ( .MILLI., .METRE. ) );
#4803 = PRODUCT_DEFINITION ( 'UNKNOWN', '', #5744, #1693 ) ;
#4804 = CARTESIAN_POINT ( 'NONE',  ( 67.00000000000000000, 1.224646799147353207E-16, -8.500000000000000000 ) ) ;
#4805 = PRODUCT_DEFINITION_SHAPE ( 'NONE', 'NONE',  #5979 ) ;
#4806 = FACE_OUTER_BOUND ( 'NONE', #3239, .T. ) ;
#4807 = ORIENTED_EDGE ( 'NONE', *, *, #2483, .T. ) ;
#4808 = ORIENTED_EDGE ( 'NONE', *, *, #4928, .F. ) ;
#4809 = SURFACE_SIDE_STYLE ('',( #2037 ) ) ;
#4810 = EDGE_CURVE ( 'NONE', #5067, #1750, #5152, .T. ) ;
#4811 = CARTESIAN_POINT ( 'NONE',  ( 34.85000000000000853, 6.612904002189975595E-15, 65.00000000000000000 ) ) ;
#4812 = ORIENTED_EDGE ( 'NONE', *, *, #2289, .F. ) ;
#4813 = AXIS2_PLACEMENT_3D ( 'NONE', #1456, #1005, #5737 ) ;
#4814 = CARTESIAN_POINT ( 'NONE',  ( 162.5000000000000000, 15.00000000000000000, -75.00000000000000000 ) ) ;
#4815 = DIRECTION ( 'NONE',  ( 1.000000000000000000, 0.000000000000000000, 0.000000000000000000 ) ) ;
#4816 = DIRECTION ( 'NONE',  ( 0.000000000000000000, 0.000000000000000000, -1.000000000000000000 ) ) ;
#4817 = ORIENTED_EDGE ( 'NONE', *, *, #2764, .F. ) ;
#4818 = CARTESIAN_POINT ( 'NONE',  ( 62.50000000000001421, -1.951563910473909559E-15, 75.00000000000000000 ) ) ;
#4819 = DIRECTION ( 'NONE',  ( 0.000000000000000000, 0.000000000000000000, 1.000000000000000000 ) ) ;
#4820 = LINE ( 'NONE', #5279, #5727 ) ;
#4821 = CARTESIAN_POINT ( 'NONE',  ( 25.00000000000000711, -6.999999999999989342, 75.00000000000000000 ) ) ;
#4822 = CARTESIAN_POINT ( 'NONE',  ( 162.4999999999999716, -6.999999999999985789, -75.00000000000000000 ) ) ;
#4823 = CARTESIAN_POINT ( 'NONE',  ( 75.00000000000001421, -15.00000000000000355, 75.00000000000000000 ) ) ;
#4824 = VERTEX_POINT ( 'NONE', #781 ) ;
#4825 = CIRCLE ( 'NONE', #4243, 4.999999999999990230 ) ;
#4826 = EDGE_LOOP ( 'NONE', ( #2093, #4007, #3312, #3552 ) ) ;
#4827 =( REPRESENTATION_RELATIONSHIP ('NONE','NONE', #5609, #2622 ) REPRESENTATION_RELATIONSHIP_WITH_TRANSFORMATION ( #5673 )SHAPE_REPRESENTATION_RELATIONSHIP( ) );
#4828 = CARTESIAN_POINT ( 'NONE',  ( -45.00000000000001421, 30.00000000000000355, -55.00000000000000000 ) ) ;
#4829 = UNCERTAINTY_MEASURE_WITH_UNIT (LENGTH_MEASURE( 1.000000000000000082E-05 ), #2155, 'distance_accuracy_value', 'NONE');
#4830 = ORIENTED_EDGE ( 'NONE', *, *, #1389, .T. ) ;
#4831 = DIRECTION ( 'NONE',  ( 0.000000000000000000, 0.000000000000000000, 1.000000000000000000 ) ) ;
#4832 = DIRECTION ( 'NONE',  ( 1.000000000000000000, -3.469446951953614189E-16, -0.000000000000000000 ) ) ;
#4833 = DIRECTION ( 'NONE',  ( -0.000000000000000000, 0.000000000000000000, 1.000000000000000000 ) ) ;
#4834 = ORIENTED_EDGE ( 'NONE', *, *, #864, .T. ) ;
#4835 = ORIENTED_EDGE ( 'NONE', *, *, #3788, .F. ) ;
#4836 = EDGE_CURVE ( 'NONE', #4171, #2259, #4497, .T. ) ;
#4837 = CIRCLE ( 'NONE', #1919, 1.336466033005844434 ) ;
#4838 = DIRECTION ( 'NONE',  ( 1.000000000000000000, -0.000000000000000000, -0.000000000000000000 ) ) ;
#4839 = ORIENTED_EDGE ( 'NONE', *, *, #2979, .T. ) ;
#4840 = ADVANCED_FACE ( 'NONE', ( #3548 ), #427, .T. ) ;
#4841 = DIRECTION ( 'NONE',  ( -1.000000000000000000, 0.000000000000000000, -0.000000000000000000 ) ) ;
#4842 = LINE ( 'NONE', #4392, #689 ) ;
#4843 = CARTESIAN_POINT ( 'NONE',  ( 2.740000000000000213, 0.000000000000000000, 0.000000000000000000 ) ) ;
#4844 = ORIENTED_EDGE ( 'NONE', *, *, #906, .F. ) ;
#4845 = CIRCLE ( 'NONE', #4063, 5.000000000000004441 ) ;
#4846 = ADVANCED_FACE ( 'NONE', ( #3572 ), #5875, .F. ) ;
#4847 = PRODUCT ( 'piston', 'piston', '', ( #2534 ) ) ;
#4848 = APPLICATION_PROTOCOL_DEFINITION ( 'draft international standard', 'automotive_design', 1998, #5950 ) ;
#4849 = CARTESIAN_POINT ( 'NONE',  ( 2.740000000000000213, -0.5149999999999973488, -0.6774776749089248540 ) ) ;
#4850 = DIRECTION ( 'NONE',  ( 0.000000000000000000, 1.000000000000000000, 0.000000000000000000 ) ) ;
#4851 = CIRCLE ( 'NONE', #5813, 5.000000000000004441 ) ;
#4852 = DIRECTION ( 'NONE',  ( 1.000000000000000000, 0.000000000000000000, -0.000000000000000000 ) ) ;
#4853 = CARTESIAN_POINT ( 'NONE',  ( -40.66987298107780902, 40.00000000000000000, 52.49999999999999289 ) ) ;
#4854 = CARTESIAN_POINT ( 'NONE',  ( 62.50000000000001421, -1.951563910473909559E-15, -55.00000000000000000 ) ) ;
#4855 = VERTEX_POINT ( 'NONE', #750 ) ;
#4856 = EDGE_CURVE ( 'NONE', #1175, #736, #2518, .T. ) ;
#4858 = EDGE_LOOP ( 'NONE', ( #4529, #4720 ) ) ;
#4857 = PRODUCT_DEFINITION_SHAPE ( 'NONE', 'NONE',  #5986 ) ;
#4859 = SURFACE_STYLE_FILL_AREA ( #3876 ) ;
#4860 = CIRCLE ( 'NONE', #3697, 0.9999999999999991118 ) ;
#4861 = DIRECTION ( 'NONE',  ( 1.000000000000000000, -0.000000000000000000, -0.000000000000000000 ) ) ;
#4862 = EDGE_LOOP ( 'NONE', ( #3842, #885 ) ) ;
#4863 = VECTOR ( 'NONE', #954, 1000.000000000000000 ) ;
#4864 = CIRCLE ( 'NONE', #4377, 2.649999999999999467 ) ;
#4865 = CARTESIAN_POINT ( 'NONE',  ( 162.5000000000000000, 15.00000000000000000, -65.00000000000000000 ) ) ;
#4866 = VECTOR ( 'NONE', #1343, 1000.000000000000000 ) ;
#4867 = AXIS2_PLACEMENT_3D ( 'NONE', #5093, #5145, #2290 ) ;
#4868 = PLANE ( 'NONE',  #4560 ) ;
#4869 = ORIENTED_EDGE ( 'NONE', *, *, #673, .F. ) ;
#4870 = CIRCLE ( 'NONE', #3412, 5.000000000000000000 ) ;
#4871 = ORIENTED_EDGE ( 'NONE', *, *, #2460, .T. ) ;
#4872 = DIRECTION ( 'NONE',  ( 1.000000000000000000, 0.000000000000000000, 0.000000000000000000 ) ) ;
#4873 = AXIS2_PLACEMENT_3D ( 'NONE', #436, #4401, #2737 ) ;
#4874 = AXIS2_PLACEMENT_3D ( 'NONE', #1029, #3282, #2396 ) ;
#4875 = AXIS2_PLACEMENT_3D ( 'NONE', #5243, #2085, #1633 ) ;
#4876 = CARTESIAN_POINT ( 'NONE',  ( 3.700000000000000178, 3.306546357697853733E-16, -2.700000000000000178 ) ) ;
#4877 = EDGE_CURVE ( 'NONE', #4354, #5437, #1917, .T. ) ;
#4878 = EDGE_LOOP ( 'NONE', ( #3299, #1300 ) ) ;
#4879 = DIRECTION ( 'NONE',  ( -0.000000000000000000, -0.000000000000000000, 1.000000000000000000 ) ) ;
#4880 = DIRECTION ( 'NONE',  ( -0.000000000000000000, -1.000000000000000000, -0.000000000000000000 ) ) ;
#4881 = AXIS2_PLACEMENT_3D ( 'NONE', #1258, #5417, #4121 ) ;
#4882 = ADVANCED_FACE ( 'NONE', ( #3723 ), #1387, .T. ) ;
#4883 = CARTESIAN_POINT ( 'NONE',  ( 196.6421356237309510, 0.000000000000000000, 5.000000000000000000 ) ) ;
#4884 = ORIENTED_EDGE ( 'NONE', *, *, #2088, .T. ) ;
#4885 = PRESENTATION_LAYER_ASSIGNMENT (  '', '', ( #4595 ) ) ;
#4886 = CARTESIAN_POINT ( 'NONE',  ( 78.30000000000001137, -6.938893903907228378E-15, -9.500000000000015987 ) ) ;
#4887 = EDGE_CURVE ( 'NONE', #1461, #1037, #5124, .T. ) ;
#4888 = FACE_OUTER_BOUND ( 'NONE', #2404, .T. ) ;
#4889 = CARTESIAN_POINT ( 'NONE',  ( 1.794155980045911036, 0.000000000000000000, 4.749999999999999112 ) ) ;
#4890 = AXIS2_PLACEMENT_3D ( 'NONE', #1565, #3419, #1984 ) ;
#4891 = DIRECTION ( 'NONE',  ( -1.000000000000000000, -0.000000000000000000, -0.000000000000000000 ) ) ;
#4892 = CARTESIAN_POINT ( 'NONE',  ( 0.5000000000000000000, 0.2499999999999982792, -1.911797424705720339 ) ) ;
#4893 = CARTESIAN_POINT ( 'NONE',  ( 25.00000000000000711, -6.999999999999988454, 65.00000000000000000 ) ) ;
#4894 = ORIENTED_EDGE ( 'NONE', *, *, #5803, .F. ) ;
#4895 = ORIENTED_EDGE ( 'NONE', *, *, #2725, .F. ) ;
#4896 = CONICAL_SURFACE ( 'NONE', #3624, 1.886264737416298409, 0.08726646259971679309 ) ;
#4897 = CARTESIAN_POINT ( 'NONE',  ( 162.4999999999999716, 7.000000000000013323, -75.00000000000000000 ) ) ;
#4898 = EDGE_CURVE ( 'NONE', #3717, #52, #5156, .T. ) ;
#4899 = ORIENTED_EDGE ( 'NONE', *, *, #5604, .T. ) ;
#4900 = LINE ( 'NONE', #3068, #417 ) ;
#4901 = CARTESIAN_POINT ( 'NONE',  ( 0.000000000000000000, 40.00000000000000000, 0.000000000000000000 ) ) ;
#4902 = CLOSED_SHELL ( 'NONE', ( #5695, #2840, #945, #4226, #93, #2344, #4257, #3259, #5582, #1396, #617, #5169, #4693 ) ) ;
#4903 = DIRECTION ( 'NONE',  ( 0.000000000000000000, 0.000000000000000000, -1.000000000000000000 ) ) ;
#4904 = ORIENTED_EDGE ( 'NONE', *, *, #3835, .F. ) ;
#4905 = VERTEX_POINT ( 'NONE', #904 ) ;
#4906 = DIRECTION ( 'NONE',  ( -0.000000000000000000, -0.000000000000000000, -1.000000000000000000 ) ) ;
#4907 = SURFACE_SIDE_STYLE ('',( #2677 ) ) ;
#4908 = VERTEX_POINT ( 'NONE', #2759 ) ;
#4909 = DIRECTION ( 'NONE',  ( 0.000000000000000000, 0.000000000000000000, 1.000000000000000000 ) ) ;
#4910 = DIRECTION ( 'NONE',  ( 0.000000000000000000, 0.000000000000000000, -1.000000000000000000 ) ) ;
#4911 = ORIENTED_EDGE ( 'NONE', *, *, #1120, .T. ) ;
#4912 = DIRECTION ( 'NONE',  ( 0.000000000000000000, 0.000000000000000000, -1.000000000000000000 ) ) ;
#4913 = ORIENTED_EDGE ( 'NONE', *, *, #2456, .T. ) ;
#4914 = AXIS2_PLACEMENT_3D ( 'NONE', #5904, #4618, #5017 ) ;
#4915 = APPLICATION_PROTOCOL_DEFINITION ( 'draft international standard', 'automotive_design', 1998, #5027 ) ;
#4916 = CARTESIAN_POINT ( 'NONE',  ( 0.06760930072668842883, -0.5149999999999961275, -0.9010842325122929708 ) ) ;
#4917 = FACE_OUTER_BOUND ( 'NONE', #2452, .T. ) ;
#4918 = DIRECTION ( 'NONE',  ( -0.000000000000000000, -1.000000000000000000, -0.000000000000000000 ) ) ;
#4919 = PRODUCT_DEFINITION_CONTEXT ( 'detailed design', #4712, 'design' ) ;
#4920 = CARTESIAN_POINT ( 'NONE',  ( 40.00000000000000711, 6.594534300202765954E-15, -55.00000000000000000 ) ) ;
#4921 = DIRECTION ( 'NONE',  ( -0.000000000000000000, -0.000000000000000000, 1.000000000000000000 ) ) ;
#4922 = ORIENTED_EDGE ( 'NONE', *, *, #5921, .F. ) ;
#4923 = EDGE_CURVE ( 'NONE', #4439, #1983, #3693, .T. ) ;
#4924 = FACE_OUTER_BOUND ( 'NONE', #2151, .T. ) ;
#4925 = ORIENTED_EDGE ( 'NONE', *, *, #5234, .F. ) ;
#4926 = AXIS2_PLACEMENT_3D ( 'NONE', #1806, #4086, #2663 ) ;
#4927 = FILL_AREA_STYLE_COLOUR ( '', #3032 ) ;
#4928 = EDGE_CURVE ( 'NONE', #3739, #4799, #474, .T. ) ;
#4929 = DIRECTION ( 'NONE',  ( 0.000000000000000000, 1.000000000000000000, -0.000000000000000000 ) ) ;
#4930 = CARTESIAN_POINT ( 'NONE',  ( 24.99999999999998224, 6.999999999999985789, 65.00000000000000000 ) ) ;
#4931 = ORIENTED_EDGE ( 'NONE', *, *, #599, .F. ) ;
#4932 = ORIENTED_EDGE ( 'NONE', *, *, #719, .T. ) ;
#4933 = FILL_AREA_STYLE ('',( #1188 ) ) ;
#4934 = CARTESIAN_POINT ( 'NONE',  ( 2.740000000000000213, 0.000000000000000000, 0.000000000000000000 ) ) ;
#4935 = ORIENTED_EDGE ( 'NONE', *, *, #5372, .F. ) ;
#4936 = DIRECTION ( 'NONE',  ( 1.000000000000000000, 0.000000000000000000, 0.000000000000000000 ) ) ;
#4937 = DIRECTION ( 'NONE',  ( 0.000000000000000000, 0.000000000000000000, 1.000000000000000000 ) ) ;
#4938 = ORIENTED_EDGE ( 'NONE', *, *, #4630, .F. ) ;
#4939 = LINE ( 'NONE', #3114, #2524 ) ;
#4940 = EDGE_LOOP ( 'NONE', ( #5763, #548, #3341, #5601 ) ) ;
#4941 = CARTESIAN_POINT ( 'NONE',  ( 55.00000000000000711, 0.000000000000000000, 0.000000000000000000 ) ) ;
#4942 = CARTESIAN_POINT ( 'NONE',  ( 150.0000000000000284, 0.000000000000000000, 45.00000000000000000 ) ) ;
#4943 = APPLICATION_CONTEXT ( 'automotive_design' ) ;
#4944 = CARTESIAN_POINT ( 'NONE',  ( 137.4999999999999716, 15.00000000000000000, -75.00000000000000000 ) ) ;
#4945 = DIRECTION ( 'NONE',  ( -0.000000000000000000, 1.000000000000000000, -0.000000000000000000 ) ) ;
#4946 = CARTESIAN_POINT ( 'NONE',  ( 0.000000000000000000, 0.000000000000000000, 65.00000000000000000 ) ) ;
#4947 = VECTOR ( 'NONE', #3921, 1000.000000000000000 ) ;
#4948 = EDGE_LOOP ( 'NONE', ( #3075, #1683, #5771, #217 ) ) ;
#4949 = CARTESIAN_POINT ( 'NONE',  ( -45.00000000000001421, 30.00000000000000355, 45.00000000000000000 ) ) ;
#4950=STYLED_ITEM('',(#6013),#126);
#4951 = AXIS2_PLACEMENT_3D ( 'NONE', #5958, #4203, #2798 ) ;
#4952 = ORIENTED_EDGE ( 'NONE', *, *, #1344, .F. ) ;
#4953 = EDGE_CURVE ( 'NONE', #1083, #853, #2237, .T. ) ;
#4954 = DIRECTION ( 'NONE',  ( 0.000000000000000000, 1.000000000000000000, 0.000000000000000000 ) ) ;
#4955 = ADVANCED_FACE ( 'NONE', ( #4183 ), #4152, .F. ) ;
#4956 = COLOUR_RGB ( '',1.000000000000000000, 0.9490196078431372140, 0.9098039215686274384 ) ;
#4957 = AXIS2_PLACEMENT_3D ( 'NONE', #1644, #4011, #3493 ) ;
#4958 = CARTESIAN_POINT ( 'NONE',  ( 75.00000000000001421, 0.000000000000000000, -10.59999999999999787 ) ) ;
#4959 = EDGE_CURVE ( 'NONE', #674, #4267, #2810, .T. ) ;
#4960 = VECTOR ( 'NONE', #391, 1000.000000000000000 ) ;
#4961 = DIRECTION ( 'NONE',  ( -1.000000000000000000, 0.000000000000000000, 0.000000000000000000 ) ) ;
#4962 = EDGE_LOOP ( 'NONE', ( #4324, #2711, #4424, #1529 ) ) ;
#4963 = ORIENTED_EDGE ( 'NONE', *, *, #4406, .T. ) ;
#4964 = AXIS2_PLACEMENT_3D ( 'NONE', #1595, #5657, #3447 ) ;
#4965 = AXIS2_PLACEMENT_3D ( 'NONE', #2967, #245, #1203 ) ;
#4966 =( NAMED_UNIT ( * ) SI_UNIT ( $, .STERADIAN. ) SOLID_ANGLE_UNIT ( ) );
#4967 = PRESENTATION_STYLE_ASSIGNMENT (( #2654 ) ) ;
#4968 = ORIENTED_EDGE ( 'NONE', *, *, #4779, .T. ) ;
#4969 = VECTOR ( 'NONE', #5370, 1000.000000000000000 ) ;
#4970 = CIRCLE ( 'NONE', #3988, 0.8509999999999999787 ) ;
#4971 = CARTESIAN_POINT ( 'NONE',  ( -49.33012701892221230, 45.00000000000000000, 52.49999999999999289 ) ) ;
#4972 = EDGE_CURVE ( 'NONE', #5207, #3560, #5544, .T. ) ;
#4973 = DIRECTION ( 'NONE',  ( -1.000000000000000000, -0.000000000000000000, -0.000000000000000000 ) ) ;
#4974 = EDGE_LOOP ( 'NONE', ( #5650, #4708 ) ) ;
#4975 = CARTESIAN_POINT ( 'NONE',  ( 2.740000000000000213, 1.042174426074397490E-16, -0.8509999999999999787 ) ) ;
#4976 = ORIENTED_EDGE ( 'NONE', *, *, #1612, .F. ) ;
#4977 = AXIS2_PLACEMENT_3D ( 'NONE', #3670, #5523, #2424 ) ;
#4978 = ITEM_DEFINED_TRANSFORMATION ( 'NONE', 'NONE', #5368,  #5080 ) ;
#4979 = AXIS2_PLACEMENT_3D ( 'NONE', #1700, #1726, #3133 ) ;
#4980 = FACE_OUTER_BOUND ( 'NONE', #4551, .T. ) ;
#4981 = AXIS2_PLACEMENT_3D ( 'NONE', #1716, #2593, #362 ) ;
#4982 = DIRECTION ( 'NONE',  ( 1.000000000000000000, 0.000000000000000000, 0.000000000000000000 ) ) ;
#4983 = LINE ( 'NONE', #2596, #502 ) ;
#4984 = DIRECTION ( 'NONE',  ( -0.000000000000000000, 0.000000000000000000, 1.000000000000000000 ) ) ;
#4985 = VERTEX_POINT ( 'NONE', #1411 ) ;
#4986 = PRESENTATION_STYLE_ASSIGNMENT (( #5045 ) ) ;
#4987 = DIRECTION ( 'NONE',  ( 0.000000000000000000, -0.000000000000000000, -1.000000000000000000 ) ) ;
#4988 = EDGE_LOOP ( 'NONE', ( #2760, #2754, #5889, #3497, #4728 ) ) ;
#4989 = DIRECTION ( 'NONE',  ( -0.000000000000000000, -0.000000000000000000, 1.000000000000000000 ) ) ;
#4990 = CIRCLE ( 'NONE', #2359, 2.500000000000000000 ) ;
#4991 = FACE_OUTER_BOUND ( 'NONE', #1453, .T. ) ;
#4992 = AXIS2_PLACEMENT_3D ( 'NONE', #2507, #1698, #3432 ) ;
#4993 = SURFACE_SIDE_STYLE ('',( #3135 ) ) ;
#4994 = DIRECTION ( 'NONE',  ( 1.000000000000000000, 0.000000000000000000, 0.000000000000000000 ) ) ;
#4995 = EDGE_CURVE ( 'NONE', #554, #726, #3, .T. ) ;
#4996 = LINE ( 'NONE', #3557, #2811 ) ;
#4998 = ORIENTED_EDGE ( 'NONE', *, *, #2316, .T. ) ;
#4997 = ADVANCED_FACE ( 'NONE', ( #507 ), #2356, .T. ) ;
#4999 = VERTEX_POINT ( 'NONE', #5180 ) ;
#5000 = DIRECTION ( 'NONE',  ( -1.000000000000000000, 0.000000000000000000, -0.000000000000000000 ) ) ;
#5001 = AXIS2_PLACEMENT_3D ( 'NONE', #3709, #1398, #5000 ) ;
#5002 = SURFACE_STYLE_FILL_AREA ( #5384 ) ;
#5003 = ORIENTED_EDGE ( 'NONE', *, *, #1900, .F. ) ;
#5004 = DIRECTION ( 'NONE',  ( -0.000000000000000000, 1.000000000000000000, -0.000000000000000000 ) ) ;
#5005 = CARTESIAN_POINT ( 'NONE',  ( 1.424271237134740131, 5.698459981794101142E-16, -4.556291390728477886 ) ) ;
#5006 = ORIENTED_EDGE ( 'NONE', *, *, #1617, .T. ) ;
#5007 = CARTESIAN_POINT ( 'NONE',  ( 224.9999999999999716, -7.000000000000015987, 75.00000000000000000 ) ) ;
#5008 = EDGE_LOOP ( 'NONE', ( #2457, #5580, #3799, #1285 ) ) ;
#5009 = CARTESIAN_POINT ( 'NONE',  ( 1.299999999999999156, 0.000000000000000000, 0.000000000000000000 ) ) ;
#5010 = EDGE_CURVE ( 'NONE', #3852, #3408, #4240, .T. ) ;
#5011 = CARTESIAN_POINT ( 'NONE',  ( -45.00000000000001421, 30.00000000000000355, 45.00000000000000000 ) ) ;
#5012 = CARTESIAN_POINT ( 'NONE',  ( 43.00000000000000000, 6.288372600415927295E-15, 75.00000000000000000 ) ) ;
#5013 = CARTESIAN_POINT ( 'NONE',  ( 135.4999999999999716, 0.000000000000000000, 0.000000000000000000 ) ) ;
#5014 = CARTESIAN_POINT ( 'NONE',  ( -40.66987298107780902, 45.00000000000000000, 52.49999999999999289 ) ) ;
#5015 = EDGE_LOOP ( 'NONE', ( #3455, #4129, #3563 ) ) ;
#5016 = SHAPE_REPRESENTATION ( 'slotted pan head screw_iso_ISO 1580 - M2 x 8 - 8N', ( #5080 ), #4395 ) ;
#5017 = DIRECTION ( 'NONE',  ( 0.000000000000000000, 0.000000000000000000, -1.000000000000000000 ) ) ;
#5018 = AXIS2_PLACEMENT_3D ( 'NONE', #3362, #87, #1921 ) ;
#5019 = ORIENTED_EDGE ( 'NONE', *, *, #320, .T. ) ;
#5020 = PLANE ( 'NONE',  #4683 ) ;
#5021 =( NAMED_UNIT ( * ) PLANE_ANGLE_UNIT ( ) SI_UNIT ( $, .RADIAN. ) );
#5022 = CARTESIAN_POINT ( 'NONE',  ( 75.00000000000001421, 1.224646799147354440E-16, 10.49999999999999822 ) ) ;
#5023 = LINE ( 'NONE', #317, #1742 ) ;
#5024 = ORIENTED_EDGE ( 'NONE', *, *, #5647, .T. ) ;
#5025 = ORIENTED_EDGE ( 'NONE', *, *, #2662, .T. ) ;
#5026 = DIRECTION ( 'NONE',  ( 0.8949343913984143528, 0.4461977533474922875, 0.000000000000000000 ) ) ;
#5027 = APPLICATION_CONTEXT ( 'automotive_design' ) ;
#5028 = DIRECTION ( 'NONE',  ( 0.8949343913984143528, -1.699539276894113739E-15, 0.4461977533474921764 ) ) ;
#5029 = ORIENTED_EDGE ( 'NONE', *, *, #753, .F. ) ;
#5030 = CARTESIAN_POINT ( 'NONE',  ( 65.15000000000001990, -1.951563910473909559E-15, 71.29999999999999716 ) ) ;
#5031 = DIRECTION ( 'NONE',  ( -0.8571673013836870192, 0.000000000000000000, -0.5150380737757234151 ) ) ;
#5032 = EDGE_CURVE ( 'NONE', #94, #2045, #1435, .T. ) ;
#5033 = ORIENTED_EDGE ( 'NONE', *, *, #2195, .T. ) ;
#5034 = DIRECTION ( 'NONE',  ( 0.000000000000000000, 1.000000000000000000, 0.000000000000000000 ) ) ;
#5035 = ADVANCED_FACE ( 'NONE', ( #1470 ), #2841, .F. ) ;
#5036 = EDGE_LOOP ( 'NONE', ( #955, #4330, #739, #5709 ) ) ;
#5037 = DIRECTION ( 'NONE',  ( 0.000000000000000000, 0.000000000000000000, -1.000000000000000000 ) ) ;
#5038 = ADVANCED_FACE ( 'NONE', ( #5625 ), #3333, .F. ) ;
#5039 = DIRECTION ( 'NONE',  ( -1.000000000000000000, -0.000000000000000000, -0.000000000000000000 ) ) ;
#5040 = AXIS2_PLACEMENT_3D ( 'NONE', #811, #4519, #1321 ) ;
#5041 = LINE ( 'NONE', #1719, #3776 ) ;
#5042 = CARTESIAN_POINT ( 'NONE',  ( 0.000000000000000000, 2.310008073021392480E-16, 1.886264737416298409 ) ) ;
#5043 = DIRECTION ( 'NONE',  ( 0.000000000000000000, 0.000000000000000000, -1.000000000000000000 ) ) ;
#5044 = VERTEX_POINT ( 'NONE', #3219 ) ;
#5045 = SURFACE_STYLE_USAGE ( .BOTH. , #3093 ) ;
#5046 = FACE_OUTER_BOUND ( 'NONE', #4099, .T. ) ;
#5047 = CIRCLE ( 'NONE', #4460, 7.864440107515625833 ) ;
#5048 = ORIENTED_EDGE ( 'NONE', *, *, #1308, .T. ) ;
#5049 = LINE ( 'NONE', #5948, #2056 ) ;
#5050 = EDGE_CURVE ( 'NONE', #3605, #1563, #3112, .T. ) ;
#5051 = AXIS2_PLACEMENT_3D ( 'NONE', #2399, #4260, #3652 ) ;
#5052 = CYLINDRICAL_SURFACE ( 'NONE', #3994, 2.649999999999999467 ) ;
#5053 = PLANE ( 'NONE',  #5613 ) ;
#5054 = CIRCLE ( 'NONE', #3213, 2.700000000000000178 ) ;
#5055 = ORIENTED_EDGE ( 'NONE', *, *, #2992, .T. ) ;
#5056 = ORIENTED_EDGE ( 'NONE', *, *, #5318, .T. ) ;
#5057 = CARTESIAN_POINT ( 'NONE',  ( 2.740000000000000213, 0.9838866223910001096, -0.5150000000000001243 ) ) ;
#5058=STYLED_ITEM('',(#6006),#196);
#5059 = AXIS2_PLACEMENT_3D ( 'NONE', #1433, #4636, #472 ) ;
#5060 = DIRECTION ( 'NONE',  ( 1.000000000000000000, -0.000000000000000000, -0.000000000000000000 ) ) ;
#5061 = ORIENTED_EDGE ( 'NONE', *, *, #1022, .F. ) ;
#5062 = CARTESIAN_POINT ( 'NONE',  ( -45.00000000000001421, 50.00000000000000000, 45.00000000000000000 ) ) ;
#5063 = LINE ( 'NONE', #1859, #2245 ) ;
#5064 = AXIS2_PLACEMENT_3D ( 'NONE', #1990, #661, #2907 ) ;
#5065 = ORIENTED_EDGE ( 'NONE', *, *, #5182, .T. ) ;
#5066 = DIRECTION ( 'NONE',  ( 1.000000000000000000, -0.000000000000000000, -0.000000000000000000 ) ) ;
#5067 = VERTEX_POINT ( 'NONE', #2933 ) ;
#5068 = ADVANCED_FACE ( 'NONE', ( #2494 ), #5713, .T. ) ;
#5069 = AXIS2_PLACEMENT_3D ( 'NONE', #5757, #2997, #3453 ) ;
#5070 = VECTOR ( 'NONE', #1253, 1000.000000000000000 ) ;
#5071 = DIRECTION ( 'NONE',  ( 0.000000000000000000, 0.000000000000000000, 1.000000000000000000 ) ) ;
#5072 = EDGE_CURVE ( 'NONE', #342, #1588, #1131, .T. ) ;
#5073 = DIRECTION ( 'NONE',  ( 4.770489558936220126E-17, 1.000000000000000000, -0.000000000000000000 ) ) ;
#5074 = DIRECTION ( 'NONE',  ( -1.000000000000000000, 0.000000000000000000, 0.000000000000000000 ) ) ;
#5075 = DIRECTION ( 'NONE',  ( 3.469446951953614189E-16, 1.000000000000000000, -1.734723475976808327E-16 ) ) ;
#5076 = ORIENTED_EDGE ( 'NONE', *, *, #4923, .F. ) ;
#5077 = AXIS2_PLACEMENT_3D ( 'NONE', #2232, #3547, #3062 ) ;
#5078 = EDGE_CURVE ( 'NONE', #2949, #1327, #4753, .T. ) ;
#5079 = DIRECTION ( 'NONE',  ( 0.000000000000000000, 0.000000000000000000, 1.000000000000000000 ) ) ;
#5080 = AXIS2_PLACEMENT_3D ( 'NONE', #3527, #4831, #667 ) ;
#5081 = FACE_OUTER_BOUND ( 'NONE', #1960, .T. ) ;
#5082 =( GEOMETRIC_REPRESENTATION_CONTEXT ( 3 ) GLOBAL_UNCERTAINTY_ASSIGNED_CONTEXT ( ( #637 ) ) GLOBAL_UNIT_ASSIGNED_CONTEXT ( ( #2820, #2392, #571 ) ) REPRESENTATION_CONTEXT ( 'NONE', 'WORKASPACE' ) );
#5083 = CARTESIAN_POINT ( 'NONE',  ( 1.849560077140141257, 0.7556913915602415655, -0.5150000000000000133 ) ) ;
#5084 = EDGE_CURVE ( 'NONE', #2949, #2312, #1172, .T. ) ;
#5085 =( GEOMETRIC_REPRESENTATION_CONTEXT ( 3 ) GLOBAL_UNCERTAINTY_ASSIGNED_CONTEXT ( ( #1747 ) ) GLOBAL_UNIT_ASSIGNED_CONTEXT ( ( #5783, #3476, #2106 ) ) REPRESENTATION_CONTEXT ( 'NONE', 'WORKASPACE' ) );
#5086 = AXIS2_PLACEMENT_3D ( 'NONE', #1356, #1724, #818 ) ;
#5087 = ORIENTED_EDGE ( 'NONE', *, *, #5908, .T. ) ;
#5088 = CIRCLE ( 'NONE', #3716, 1.099999999999998535 ) ;
#5089 = CARTESIAN_POINT ( 'NONE',  ( 66.39913938277356920, 0.000000000000000000, 9.500000000000000000 ) ) ;
#5090 = LINE ( 'NONE', #3261, #3389 ) ;
#5091 = ORIENTED_EDGE ( 'NONE', *, *, #4800, .T. ) ;
#5092 = CARTESIAN_POINT ( 'NONE',  ( 65.00000000000001421, -1.645402210687070900E-15, -65.00000000000000000 ) ) ;
#5093 = CARTESIAN_POINT ( 'NONE',  ( 196.6421356237309510, 0.000000000000000000, 0.000000000000000000 ) ) ;
#5094 = VERTEX_POINT ( 'NONE', #1626 ) ;
#5095 = ORIENTED_EDGE ( 'NONE', *, *, #1465, .F. ) ;
#5096 = FACE_OUTER_BOUND ( 'NONE', #2428, .T. ) ;
#5097 = FACE_OUTER_BOUND ( 'NONE', #3578, .T. ) ;
#5098 = DIRECTION ( 'NONE',  ( 0.000000000000000000, 1.000000000000000000, 0.000000000000000000 ) ) ;
#5099 = CARTESIAN_POINT ( 'NONE',  ( 0.000000000000000000, 0.5149999999999917977, 2.350000000000001865 ) ) ;
#5100 = CARTESIAN_POINT ( 'NONE',  ( 67.00000000000001421, 0.000000000000000000, -7.000000000000000000 ) ) ;
#5101 = ORIENTED_EDGE ( 'NONE', *, *, #4509, .T. ) ;
#5102 = DIRECTION ( 'NONE',  ( 0.9997893732277642886, 0.000000000000000000, 0.02052338132068530496 ) ) ;
#5103 = CARTESIAN_POINT ( 'NONE',  ( 37.50000000000000711, 6.288372600415927295E-15, -55.00000000000000000 ) ) ;
#5104 = LINE ( 'NONE', #2787, #228 ) ;
#5105 = EDGE_CURVE ( 'NONE', #5556, #1147, #3807, .T. ) ;
#5106 = ORIENTED_EDGE ( 'NONE', *, *, #2435, .F. ) ;
#5107 = CARTESIAN_POINT ( 'NONE',  ( 7.345657149124969365, -5.313980200056029618E-16, -1.312408941149200148 ) ) ;
#5108 = CIRCLE ( 'NONE', #1511, 0.5999999999999999778 ) ;
#5109 = EDGE_CURVE ( 'NONE', #698, #500, #498, .T. ) ;
#5110 = ORIENTED_EDGE ( 'NONE', *, *, #1612, .T. ) ;
#5111 = DIRECTION ( 'NONE',  ( 1.000000000000000000, -0.000000000000000000, -0.000000000000000000 ) ) ;
#5112 = AXIS2_PLACEMENT_3D ( 'NONE', #136, #4318, #3317 ) ;
#5113 = DIRECTION ( 'NONE',  ( -1.000000000000000000, 0.000000000000000000, -0.000000000000000000 ) ) ;
#5114 = CIRCLE ( 'NONE', #1513, 7.864440107515625833 ) ;
#5115 = DIRECTION ( 'NONE',  ( -0.000000000000000000, -0.000000000000000000, 1.000000000000000000 ) ) ;
#5116 = ORIENTED_EDGE ( 'NONE', *, *, #3351, .F. ) ;
#5117 = LINE ( 'NONE', #5561, #119 ) ;
#5118 = ORIENTED_EDGE ( 'NONE', *, *, #5032, .F. ) ;
#5119 = ORIENTED_EDGE ( 'NONE', *, *, #4555, .F. ) ;
#5120 = CARTESIAN_POINT ( 'NONE',  ( 8.000000000000000000, 0.5150000000000000133, 1.798112889504231112E-15 ) ) ;
#5121 = FACE_BOUND ( 'NONE', #2601, .T. ) ;
#5122 = DIRECTION ( 'NONE',  ( 0.000000000000000000, 0.000000000000000000, -1.000000000000000000 ) ) ;
#5123 = DIRECTION ( 'NONE',  ( -0.000000000000000000, 0.000000000000000000, 1.000000000000000000 ) ) ;
#5124 = LINE ( 'NONE', #3771, #3015 ) ;
#5125 = ORIENTED_EDGE ( 'NONE', *, *, #4972, .T. ) ;
#5126 = CARTESIAN_POINT ( 'NONE',  ( 0.000000000000000000, 0.000000000000000000, 0.000000000000000000 ) ) ;
#5127 = CARTESIAN_POINT ( 'NONE',  ( 75.00000000000001421, 0.000000000000000000, 0.000000000000000000 ) ) ;
#5128 = DIRECTION ( 'NONE',  ( 0.000000000000000000, 0.000000000000000000, 1.000000000000000000 ) ) ;
#5129 = EDGE_LOOP ( 'NONE', ( #2660, #428, #5965, #5029 ) ) ;
#5130 = DIRECTION ( 'NONE',  ( 0.000000000000000000, 0.000000000000000000, 1.000000000000000000 ) ) ;
#5131 = EDGE_CURVE ( 'NONE', #1679, #2341, #145, .T. ) ;
#5132 = EDGE_CURVE ( 'NONE', #2264, #1403, #5252, .T. ) ;
#5133 = EDGE_CURVE ( 'NONE', #3585, #3220, #5726, .T. ) ;
#5134 = AXIS2_PLACEMENT_3D ( 'NONE', #5559, #5060, #1400 ) ;
#5135 = ORIENTED_EDGE ( 'NONE', *, *, #3826, .F. ) ;
#5136 = FACE_OUTER_BOUND ( 'NONE', #4111, .T. ) ;
#5137 = EDGE_CURVE ( 'NONE', #4999, #3205, #1941, .T. ) ;
#5138 = DIRECTION ( 'NONE',  ( -1.000000000000000000, 0.000000000000000000, -0.000000000000000000 ) ) ;
#5139 = CONTEXT_DEPENDENT_SHAPE_REPRESENTATION ( #4408, #1016 ) ;
#5140 = AXIS2_PLACEMENT_3D ( 'NONE', #4545, #1538, #5247 ) ;
#5141 = PRODUCT_DEFINITION_SHAPE ( 'NONE', 'NONE',  #5989 ) ;
#5142 = VECTOR ( 'NONE', #734, 1000.000000000000114 ) ;
#5143 = DIRECTION ( 'NONE',  ( -0.000000000000000000, -0.000000000000000000, -1.000000000000000000 ) ) ;
#5144 = EDGE_LOOP ( 'NONE', ( #482, #1269, #2219, #3442 ) ) ;
#5145 = DIRECTION ( 'NONE',  ( -1.000000000000000000, -0.000000000000000000, -0.000000000000000000 ) ) ;
#5146 = ORIENTED_EDGE ( 'NONE', *, *, #3762, .F. ) ;
#5147 = ORIENTED_EDGE ( 'NONE', *, *, #5405, .F. ) ;
#5148 = CONICAL_SURFACE ( 'NONE', #205, 2.500000000000002220, 1.029744260000002631 ) ;
#5149 = CYLINDRICAL_SURFACE ( 'NONE', #2321, 12.00000000000000000 ) ;
#5150 = EDGE_CURVE ( 'NONE', #5607, #4227, #1160, .T. ) ;
#5151 = DIRECTION ( 'NONE',  ( 0.000000000000000000, 1.000000000000000000, 0.000000000000000000 ) ) ;
#5152 = CIRCLE ( 'NONE', #2035, 0.2000000000000000944 ) ;
#5153 = CIRCLE ( 'NONE', #5246, 5.000000000000000000 ) ;
#5154 = DIRECTION ( 'NONE',  ( 0.000000000000000000, 1.000000000000000000, 0.000000000000000000 ) ) ;
#5155 = FACE_OUTER_BOUND ( 'NONE', #5684, .T. ) ;
#5156 = LINE ( 'NONE', #560, #1266 ) ;
#5157 = VERTEX_POINT ( 'NONE', #2531 ) ;
#5158 = AXIS2_PLACEMENT_3D ( 'NONE', #3179, #4743, #3823 ) ;
#5159 = LINE ( 'NONE', #598, #2776 ) ;
#5160 = LINE ( 'NONE', #4275, #963 ) ;
#5162 = AXIS2_PLACEMENT_3D ( 'NONE', #4558, #1241, #788 ) ;
#5161 = DIRECTION ( 'NONE',  ( 1.000000000000000000, 0.000000000000000000, 0.000000000000000000 ) ) ;
#5163 = ORIENTED_EDGE ( 'NONE', *, *, #3862, .F. ) ;
#5164 = ORIENTED_EDGE ( 'NONE', *, *, #1973, .F. ) ;
#5165 = DIRECTION ( 'NONE',  ( 1.000000000000000000, -3.469446951953614189E-16, 0.000000000000000000 ) ) ;
#5166 = ORIENTED_EDGE ( 'NONE', *, *, #4737, .T. ) ;
#5167 = LINE ( 'NONE', #3314, #5637 ) ;
#5168 = CARTESIAN_POINT ( 'NONE',  ( 75.00000000000001421, 1.347111479062087764E-16, -8.400000000000000355 ) ) ;
#5169 = ADVANCED_FACE ( 'NONE', ( #653 ), #5231, .F. ) ;
#5170 = ORIENTED_EDGE ( 'NONE', *, *, #5405, .T. ) ;
#5171 = FACE_OUTER_BOUND ( 'NONE', #1047, .T. ) ;
#5172 = ADVANCED_FACE ( 'NONE', ( #1070 ), #204, .T. ) ;
#5173 = DIRECTION ( 'NONE',  ( 0.000000000000000000, 0.000000000000000000, -1.000000000000000000 ) ) ;
#5174 = ORIENTED_EDGE ( 'NONE', *, *, #367, .T. ) ;
#5175 = ORIENTED_EDGE ( 'NONE', *, *, #4995, .F. ) ;
#5176 =( NAMED_UNIT ( * ) PLANE_ANGLE_UNIT ( ) SI_UNIT ( $, .RADIAN. ) );
#5177 = DIRECTION ( 'NONE',  ( 0.000000000000000000, 1.000000000000000000, -0.000000000000000000 ) ) ;
#5178 = CARTESIAN_POINT ( 'NONE',  ( 0.9586399445693637444, -0.8293189044373081575, 0.5149999999999994582 ) ) ;
#5179 = CARTESIAN_POINT ( 'NONE',  ( 77.00000000000001421, 0.000000000000000000, 12.00000000000000000 ) ) ;
#5180 = CARTESIAN_POINT ( 'NONE',  ( 55.00000000000000711, 0.000000000000000000, -7.000000000000000000 ) ) ;
#5181 = ORIENTED_EDGE ( 'NONE', *, *, #2504, .T. ) ;
#5182 = EDGE_CURVE ( 'NONE', #2264, #3585, #4481, .T. ) ;
#5183 = DIRECTION ( 'NONE',  ( 1.000000000000000000, 0.000000000000000000, 0.000000000000000000 ) ) ;
#5184 = CARTESIAN_POINT ( 'NONE',  ( 35.00000000000000000, 6.594534300202765954E-15, 65.00000000000000000 ) ) ;
#5185 = VECTOR ( 'NONE', #3486, 1000.000000000000000 ) ;
#5186 = LINE ( 'NONE', #2388, #5425 ) ;
#5187 = PLANE ( 'NONE',  #1858 ) ;
#5188 = ORIENTED_EDGE ( 'NONE', *, *, #4133, .T. ) ;
#5190 = EDGE_LOOP ( 'NONE', ( #979, #1428, #2812, #585 ) ) ;
#5189 = PRODUCT_DEFINITION_SHAPE ( 'NONE', 'NONE',  #5537 ) ;
#5191 = FILL_AREA_STYLE_COLOUR ( '', #3523 ) ;
#5192 = DIRECTION ( 'NONE',  ( -0.000000000000000000, -0.000000000000000000, 1.000000000000000000 ) ) ;
#5193 = ORIENTED_EDGE ( 'NONE', *, *, #26, .T. ) ;
#5194 = DIRECTION ( 'NONE',  ( 0.000000000000000000, 0.000000000000000000, 1.000000000000000000 ) ) ;
#5195 = DIRECTION ( 'NONE',  ( -0.000000000000000000, -1.000000000000000000, -0.000000000000000000 ) ) ;
#5196 = DIRECTION ( 'NONE',  ( -1.000000000000000000, 0.000000000000000000, -0.000000000000000000 ) ) ;
#5197 = EDGE_LOOP ( 'NONE', ( #3814, #4223, #5275, #258 ) ) ;
#5198 = ORIENTED_EDGE ( 'NONE', *, *, #4138, .F. ) ;
#5199 = FACE_OUTER_BOUND ( 'NONE', #2292, .T. ) ;
#5200 = CARTESIAN_POINT ( 'NONE',  ( -45.00000000000001421, 50.00000000000000000, 39.99999999999999289 ) ) ;
#5201 = EDGE_CURVE ( 'NONE', #3189, #4444, #2635, .T. ) ;
#5202 = ORIENTED_EDGE ( 'NONE', *, *, #1985, .F. ) ;
#5203 = CARTESIAN_POINT ( 'NONE',  ( 137.4999999999999716, 15.00000000000000000, 75.00000000000001421 ) ) ;
#5204 = ADVANCED_FACE ( 'NONE', ( #1982 ), #3402, .F. ) ;
#5205 = DIRECTION ( 'NONE',  ( -0.000000000000000000, -1.000000000000000000, -0.000000000000000000 ) ) ;
#5206 = DIRECTION ( 'NONE',  ( -1.000000000000000000, -0.000000000000000000, -0.000000000000000000 ) ) ;
#5207 = VERTEX_POINT ( 'NONE', #4393 ) ;
#5208 = ADVANCED_FACE ( 'NONE', ( #5687 ), #2078, .F. ) ;
#5209 = FACE_OUTER_BOUND ( 'NONE', #5373, .T. ) ;
#5210 = FACE_OUTER_BOUND ( 'NONE', #5925, .T. ) ;
#5211 = CARTESIAN_POINT ( 'NONE',  ( 75.00000000000001421, -7.000000000000006217, -65.00000000000000000 ) ) ;
#5212 = LINE ( 'NONE', #512, #2249 ) ;
#5213 = VERTEX_POINT ( 'NONE', #5843 ) ;
#5214 = ORIENTED_EDGE ( 'NONE', *, *, #727, .F. ) ;
#5215 = DIRECTION ( 'NONE',  ( 0.000000000000000000, 0.000000000000000000, 1.000000000000000000 ) ) ;
#5216 = EDGE_CURVE ( 'NONE', #4461, #1830, #313, .T. ) ;
#5217 = FACE_OUTER_BOUND ( 'NONE', #717, .T. ) ;
#5218 = CARTESIAN_POINT ( 'NONE',  ( 24.99999999999998224, -7.000000000000006217, 75.00000000000000000 ) ) ;
#5219 = DIRECTION ( 'NONE',  ( 0.000000000000000000, 1.000000000000000000, 0.000000000000000000 ) ) ;
#5220 = VECTOR ( 'NONE', #4635, 1000.000000000000000 ) ;
#5221 = FACE_OUTER_BOUND ( 'NONE', #3064, .T. ) ;
#5222 = VERTEX_POINT ( 'NONE', #2224 ) ;
#5223 = ORIENTED_EDGE ( 'NONE', *, *, #2767, .T. ) ;
#5224 = DIRECTION ( 'NONE',  ( 0.000000000000000000, 0.000000000000000000, 1.000000000000000000 ) ) ;
#5225 = AXIS2_PLACEMENT_3D ( 'NONE', #3373, #5219, #4382 ) ;
#5226 = DIRECTION ( 'NONE',  ( 0.000000000000000000, 0.000000000000000000, 1.000000000000000000 ) ) ;
#5227 = EDGE_LOOP ( 'NONE', ( #4935, #3040, #384, #647 ) ) ;
#5228 = FACE_BOUND ( 'NONE', #4568, .T. ) ;
#5229 = LINE ( 'NONE', #624, #4081 ) ;
#5230 = PRODUCT ( 'lock', 'lock', '', ( #3026 ) ) ;
#5231 = CYLINDRICAL_SURFACE ( 'NONE', #4380, 1.099999999999998535 ) ;
#5232 = VECTOR ( 'NONE', #4473, 1000.000000000000000 ) ;
#5233 = ORIENTED_EDGE ( 'NONE', *, *, #2276, .T. ) ;
#5234 = EDGE_CURVE ( 'NONE', #4416, #5838, #2589, .T. ) ;
#5235 = APPLICATION_PROTOCOL_DEFINITION ( 'draft international standard', 'automotive_design', 1998, #2653 ) ;
#5236 = DIRECTION ( 'NONE',  ( 0.000000000000000000, 1.000000000000000000, 0.000000000000000000 ) ) ;
#5237 = EDGE_CURVE ( 'NONE', #1034, #225, #3309, .T. ) ;
#5238 = AXIS2_PLACEMENT_3D ( 'NONE', #2757, #1296, #1835 ) ;
#5239 = CARTESIAN_POINT ( 'NONE',  ( 2.740000000000000213, -0.9838866223905674557, -0.5150000000000000133 ) ) ;
#5240 = DIRECTION ( 'NONE',  ( 0.000000000000000000, -3.552713678800500929E-15, 1.000000000000000000 ) ) ;
#5241 = CARTESIAN_POINT ( 'NONE',  ( 137.4999999999999716, 6.999999999999985789, 65.00000000000000000 ) ) ;
#5242 = EDGE_CURVE ( 'NONE', #3560, #5481, #25, .T. ) ;
#5243 = CARTESIAN_POINT ( 'NONE',  ( -45.00000000000001421, 30.00000000000000355, -45.00000000000000000 ) ) ;
#5244 = ORIENTED_EDGE ( 'NONE', *, *, #578, .F. ) ;
#5245 = VECTOR ( 'NONE', #5593, 1000.000000000000000 ) ;
#5246 = AXIS2_PLACEMENT_3D ( 'NONE', #2526, #1525, #172 ) ;
#5247 = DIRECTION ( 'NONE',  ( 1.000000000000000000, 0.000000000000000000, 0.000000000000000000 ) ) ;
#5248 = PRESENTATION_STYLE_ASSIGNMENT (( #1637 ) ) ;
#5249 =( REPRESENTATION_RELATIONSHIP ('NONE','NONE', #5609, #4225 ) REPRESENTATION_RELATIONSHIP_WITH_TRANSFORMATION ( #3234 )SHAPE_REPRESENTATION_RELATIONSHIP( ) );
#5250 = CARTESIAN_POINT ( 'NONE',  ( -45.00000000000001421, 50.00000000000000000, 39.99999999999999289 ) ) ;
#5251 = UNCERTAINTY_MEASURE_WITH_UNIT (LENGTH_MEASURE( 1.000000000000000082E-05 ), #4802, 'distance_accuracy_value', 'NONE');
#5252 = CIRCLE ( 'NONE', #975, 7.983406227920510467 ) ;
#5253 = CIRCLE ( 'NONE', #5158, 0.8509999999999999787 ) ;
#5254 = ORIENTED_EDGE ( 'NONE', *, *, #2129, .T. ) ;
#5255 = VECTOR ( 'NONE', #1298, 1000.000000000000000 ) ;
#5256 = CIRCLE ( 'NONE', #2740, 5.000000000000004441 ) ;
#5257 = ADVANCED_FACE ( 'NONE', ( #1687 ), #5363, .T. ) ;
#5258 = DIRECTION ( 'NONE',  ( 0.000000000000000000, -0.000000000000000000, 1.000000000000000000 ) ) ;
#5259 = ITEM_DEFINED_TRANSFORMATION ( 'NONE', 'NONE', #1292,  #5080 ) ;
#5260 = PLANE ( 'NONE',  #5810 ) ;
#5261 = PRESENTATION_LAYER_ASSIGNMENT (  '', '', ( #3609 ) ) ;
#5262 = PRESENTATION_STYLE_ASSIGNMENT (( #4466 ) ) ;
#5263 = ORIENTED_EDGE ( 'NONE', *, *, #2693, .F. ) ;
#5264 = ORIENTED_EDGE ( 'NONE', *, *, #4323, .T. ) ;
#5265 = CARTESIAN_POINT ( 'NONE',  ( 25.00000000000000711, -6.999999999999988454, 65.00000000000000000 ) ) ;
#5266 = PRESENTATION_LAYER_ASSIGNMENT (  '', '', ( #1185 ) ) ;
#5267 = FACE_OUTER_BOUND ( 'NONE', #250, .T. ) ;
#5268 = EDGE_LOOP ( 'NONE', ( #2876, #4976, #4839, #1494 ) ) ;
#5269 = SHAPE_REPRESENTATION ( 'Reciprocating Feed Carriage Block', ( #5080 ), #2935 ) ;
#5270 = CYLINDRICAL_SURFACE ( 'NONE', #2815, 0.9999999999999991118 ) ;
#5271 = DIRECTION ( 'NONE',  ( -0.000000000000000000, -0.000000000000000000, 1.000000000000000000 ) ) ;
#5272 = MECHANICAL_DESIGN_GEOMETRIC_PRESENTATION_REPRESENTATION (  '', ( #1386 ), #1779 ) ;
#5273 = DIRECTION ( 'NONE',  ( -0.000000000000000000, -0.000000000000000000, -1.000000000000000000 ) ) ;
#5274 = AXIS2_PLACEMENT_3D ( 'NONE', #4006, #306, #1141 ) ;
#5275 = ORIENTED_EDGE ( 'NONE', *, *, #531, .T. ) ;
#5276 = DIRECTION ( 'NONE',  ( 1.000000000000000000, 0.000000000000000000, 6.123233995736766036E-17 ) ) ;
#5277 = AXIS2_PLACEMENT_3D ( 'NONE', #4681, #2454, #5215 ) ;
#5278 = CARTESIAN_POINT ( 'NONE',  ( 1.794155980045911036, 5.817072295949926440E-16, -4.749999999999999112 ) ) ;
#5279 = CARTESIAN_POINT ( 'NONE',  ( -53.66025403784439618, 40.00000000000000000, 45.00000000000001421 ) ) ;
#5280 = DIRECTION ( 'NONE',  ( -0.000000000000000000, 0.000000000000000000, 1.000000000000000000 ) ) ;
#5281 = CARTESIAN_POINT ( 'NONE',  ( -25.39999999999996305, 0.000000000000000000, 0.000000000000000000 ) ) ;
#5282 = DIRECTION ( 'NONE',  ( 0.000000000000000000, -0.000000000000000000, -1.000000000000000000 ) ) ;
#5283 = VERTEX_POINT ( 'NONE', #1656 ) ;
#5284 = AXIS2_PLACEMENT_3D ( 'NONE', #2946, #42, #2393 ) ;
#5285 = VERTEX_POINT ( 'NONE', #5007 ) ;
#5286 = FILL_AREA_STYLE_COLOUR ( '', #5939 ) ;
#5287 = DIRECTION ( 'NONE',  ( -0.000000000000000000, -0.000000000000000000, 1.000000000000000000 ) ) ;
#5288 = ORIENTED_EDGE ( 'NONE', *, *, #2180, .T. ) ;
#5289 = ADVANCED_FACE ( 'NONE', ( #3992 ), #2683, .F. ) ;
#5290 = LINE ( 'NONE', #706, #2882 ) ;
#5291 = PRODUCT_DEFINITION_SHAPE ( 'NONE', 'NONE',  #5990 ) ;
#5292 = CARTESIAN_POINT ( 'NONE',  ( 25.00000000000000711, -6.999999999999989342, 75.00000000000000000 ) ) ;
#5293 = EDGE_CURVE ( 'NONE', #4312, #2772, #4769, .T. ) ;
#5294 = ORIENTED_EDGE ( 'NONE', *, *, #5660, .T. ) ;
#5295 = EDGE_LOOP ( 'NONE', ( #2486, #4659 ) ) ;
#5296 = CIRCLE ( 'NONE', #1405, 1.037871761867652065 ) ;
#5297 = DIRECTION ( 'NONE',  ( 0.000000000000000000, 0.000000000000000000, -1.000000000000000000 ) ) ;
#5298 = ORIENTED_EDGE ( 'NONE', *, *, #4185, .F. ) ;
#5299 = CIRCLE ( 'NONE', #5112, 0.8509999999999999787 ) ;
#5300 = PLANE ( 'NONE',  #5430 ) ;
#5301 = EDGE_CURVE ( 'NONE', #2228, #3393, #1197, .T. ) ;
#5302 = DIRECTION ( 'NONE',  ( -1.000000000000000000, 0.000000000000000000, 0.000000000000000000 ) ) ;
#5303 = DIRECTION ( 'NONE',  ( 0.000000000000000000, 0.000000000000000000, -1.000000000000000000 ) ) ;
#5304 = VERTEX_POINT ( 'NONE', #3540 ) ;
#5305 = FACE_OUTER_BOUND ( 'NONE', #2235, .T. ) ;
#5306 = LINE ( 'NONE', #1598, #3403 ) ;
#5307 = LINE ( 'NONE', #1168, #1357 ) ;
#5308 = LINE ( 'NONE', #4853, #2335 ) ;
#5309 = DIRECTION ( 'NONE',  ( -0.000000000000000000, -0.000000000000000000, 1.000000000000000000 ) ) ;
#5310 = ORIENTED_EDGE ( 'NONE', *, *, #3973, .F. ) ;
#5311 = ORIENTED_EDGE ( 'NONE', *, *, #567, .F. ) ;
#5312 = SURFACE_SIDE_STYLE ('',( #3458 ) ) ;
#5313 = FACE_BOUND ( 'NONE', #856, .T. ) ;
#5314 = ORIENTED_EDGE ( 'NONE', *, *, #5647, .F. ) ;
#5315 = DIRECTION ( 'NONE',  ( 1.000000000000000000, 0.000000000000000000, 0.000000000000000000 ) ) ;
#5316 = EDGE_CURVE ( 'NONE', #2003, #3927, #383, .T. ) ;
#5317 = DIRECTION ( 'NONE',  ( -0.000000000000000000, 8.673617379884040402E-17, -1.000000000000000000 ) ) ;
#5318 = EDGE_CURVE ( 'NONE', #1962, #708, #4080, .T. ) ;
#5319 = EDGE_CURVE ( 'NONE', #2440, #475, #5389, .T. ) ;
#5320 = DIRECTION ( 'NONE',  ( 0.000000000000000000, 0.000000000000000000, -1.000000000000000000 ) ) ;
#5322 = ORIENTED_EDGE ( 'NONE', *, *, #3496, .T. ) ;
#5321 = EDGE_CURVE ( 'NONE', #2852, #5342, #4939, .T. ) ;
#5323 = VERTEX_POINT ( 'NONE', #3082 ) ;
#5324 = AXIS2_PLACEMENT_3D ( 'NONE', #2439, #3019, #1651 ) ;
#5325 = DIRECTION ( 'NONE',  ( -0.000000000000000000, -0.000000000000000000, 1.000000000000000000 ) ) ;
#5326 = VERTEX_POINT ( 'NONE', #5480 ) ;
#5327 = DIRECTION ( 'NONE',  ( 0.000000000000000000, 0.000000000000000000, 1.000000000000000000 ) ) ;
#5328 = CARTESIAN_POINT ( 'NONE',  ( 0.3226060873438383325, 0.5149999999999923528, 2.189154565102733319 ) ) ;
#5329 = APPLICATION_CONTEXT ( 'automotive_design' ) ;
#5330 = DIRECTION ( 'NONE',  ( 1.000000000000000000, 0.000000000000000000, 0.000000000000000000 ) ) ;
#5331 = ORIENTED_EDGE ( 'NONE', *, *, #405, .T. ) ;
#5332 = CIRCLE ( 'NONE', #5134, 0.9999999999999991118 ) ;
#5333 = SHAPE_DEFINITION_REPRESENTATION ( #3107, #5882 ) ;
#5334 = EDGE_CURVE ( 'NONE', #4296, #4142, #3773, .T. ) ;
#5335 = DIRECTION ( 'NONE',  ( -1.000000000000000000, -0.000000000000000000, -0.000000000000000000 ) ) ;
#5336 = FACE_OUTER_BOUND ( 'NONE', #4643, .T. ) ;
#5337 = AXIS2_PLACEMENT_3D ( 'NONE', #3960, #2568, #1664 ) ;
#5338 = FACE_BOUND ( 'NONE', #2802, .T. ) ;
#5339 = CARTESIAN_POINT ( 'NONE',  ( 0.5000000000000000000, 0.000000000000000000, 0.000000000000000000 ) ) ;
#5340 = FACE_OUTER_BOUND ( 'NONE', #3209, .T. ) ;
#5341 = ORIENTED_EDGE ( 'NONE', *, *, #3647, .F. ) ;
#5342 = VERTEX_POINT ( 'NONE', #4975 ) ;
#5343 = CIRCLE ( 'NONE', #5059, 2.649999999999999467 ) ;
#5344 = CARTESIAN_POINT ( 'NONE',  ( 77.00000000000001421, 0.000000000000000000, -10.59999999999999787 ) ) ;
#5345 = ORIENTED_EDGE ( 'NONE', *, *, #5109, .F. ) ;
#5346 = VECTOR ( 'NONE', #1574, 1000.000000000000000 ) ;
#5347 = AXIS2_PLACEMENT_3D ( 'NONE', #2995, #4850, #1663 ) ;
#5348 =( NAMED_UNIT ( * ) SI_UNIT ( $, .STERADIAN. ) SOLID_ANGLE_UNIT ( ) );
#5349 = CARTESIAN_POINT ( 'NONE',  ( 150.0000000000000284, 0.000000000000000000, -49.99999999999998579 ) ) ;
#5350 = AXIS2_PLACEMENT_3D ( 'NONE', #660, #1507, #1045 ) ;
#5351 = AXIS2_PLACEMENT_3D ( 'NONE', #2587, #1775, #3053 ) ;
#5352 = CARTESIAN_POINT ( 'NONE',  ( 25.00000000000000711, -6.999999999999988454, -65.00000000000000000 ) ) ;
#5353 = CONICAL_SURFACE ( 'NONE', #2739, 1.886264737416298409, 0.08726646259971679309 ) ;
#5354 = VERTEX_POINT ( 'NONE', #861 ) ;
#5355 = VECTOR ( 'NONE', #371, 1000.000000000000000 ) ;
#5356 = EDGE_CURVE ( 'NONE', #2658, #1436, #1317, .T. ) ;
#5357 = ORIENTED_EDGE ( 'NONE', *, *, #3953, .F. ) ;
#5358 = CARTESIAN_POINT ( 'NONE',  ( 62.50000000000001421, -1.951563910473909559E-15, -65.00000000000000000 ) ) ;
#5359 = VECTOR ( 'NONE', #1277, 1000.000000000000000 ) ;
#5360 = ORIENTED_EDGE ( 'NONE', *, *, #656, .F. ) ;
#5361 = CARTESIAN_POINT ( 'NONE',  ( -45.00000000000001421, 30.00000000000000355, 50.00000000000000000 ) ) ;
#5362 = DIRECTION ( 'NONE',  ( 1.000000000000000000, 0.000000000000000000, 0.000000000000000000 ) ) ;
#5363 = PLANE ( 'NONE',  #2922 ) ;
#5364 = EDGE_LOOP ( 'NONE', ( #438, #5563, #3091, #3430 ) ) ;
#5365 = CONTEXT_DEPENDENT_SHAPE_REPRESENTATION ( #4320, #581 ) ;
#5366 = DIRECTION ( 'NONE',  ( 0.000000000000000000, -0.000000000000000000, 1.000000000000000000 ) ) ;
#5367 = CARTESIAN_POINT ( 'NONE',  ( 68.00000000000000000, -1.951563910473909559E-15, 75.00000000000000000 ) ) ;
#5368 = AXIS2_PLACEMENT_3D ( 'NONE', #5126, #5595, #957 ) ;
#5369 = DIRECTION ( 'NONE',  ( 0.000000000000000000, 0.000000000000000000, 1.000000000000000000 ) ) ;
#5370 = DIRECTION ( 'NONE',  ( 0.9961946980917455452, 1.067350013832301058E-17, 0.08715574274765848506 ) ) ;
#5371 = CYLINDRICAL_SURFACE ( 'NONE', #5064, 1.099999999999998535 ) ;
#5372 = EDGE_CURVE ( 'NONE', #2312, #4518, #2171, .T. ) ;
#5373 = EDGE_LOOP ( 'NONE', ( #1493, #85, #5174, #1011, #4932 ) ) ;
#5374 =( NAMED_UNIT ( * ) PLANE_ANGLE_UNIT ( ) SI_UNIT ( $, .RADIAN. ) );
#5375 = CYLINDRICAL_SURFACE ( 'NONE', #1485, 2.500000000000000000 ) ;
#5376 = EDGE_LOOP ( 'NONE', ( #4334, #3658, #4079, #3471, #3142 ) ) ;
#5377 =( NAMED_UNIT ( * ) PLANE_ANGLE_UNIT ( ) SI_UNIT ( $, .RADIAN. ) );
#5378 = DIRECTION ( 'NONE',  ( 1.000000000000000000, 0.000000000000000000, 0.000000000000000000 ) ) ;
#5379 = CIRCLE ( 'NONE', #3156, 5.499999999999991118 ) ;
#5380 = CARTESIAN_POINT ( 'NONE',  ( 67.00000000000000000, 0.000000000000000000, 8.500000000000000000 ) ) ;
#5381 = CIRCLE ( 'NONE', #1891, 5.000000000000004441 ) ;
#5382 = VERTEX_POINT ( 'NONE', #1802 ) ;
#5383 = ORIENTED_EDGE ( 'NONE', *, *, #4397, .F. ) ;
#5384 = FILL_AREA_STYLE ('',( #738 ) ) ;
#5385 = ORIENTED_EDGE ( 'NONE', *, *, #3998, .T. ) ;
#5386 = CYLINDRICAL_SURFACE ( 'NONE', #3016, 7.500000000000000000 ) ;
#5387 = DIRECTION ( 'NONE',  ( 1.000000000000000000, 0.000000000000000000, 0.000000000000000000 ) ) ;
#5388 = ORIENTED_EDGE ( 'NONE', *, *, #1287, .T. ) ;
#5389 = LINE ( 'NONE', #1225, #2822 ) ;
#5390 = VERTEX_POINT ( 'NONE', #4117 ) ;
#5391 = EDGE_CURVE ( 'NONE', #283, #5323, #5508, .T. ) ;
#5392 = DIRECTION ( 'NONE',  ( 0.000000000000000000, 0.000000000000000000, 1.000000000000000000 ) ) ;
#5393 = EDGE_CURVE ( 'NONE', #3440, #5618, #3657, .T. ) ;
#5394 = CARTESIAN_POINT ( 'NONE',  ( 35.00000000000000000, 6.594534300202765954E-15, 55.00000000000000000 ) ) ;
#5395 = CARTESIAN_POINT ( 'NONE',  ( 0.000000000000000000, -0.2499999999999999445, 1.312875263449798879 ) ) ;
#5396 = CARTESIAN_POINT ( 'NONE',  ( 224.9999999999999716, 6.999999999999985789, 65.00000000000000000 ) ) ;
#5397 = DIRECTION ( 'NONE',  ( 1.000000000000000000, 0.000000000000000000, 0.000000000000000000 ) ) ;
#5398 = ORIENTED_EDGE ( 'NONE', *, *, #5319, .T. ) ;
#5399 = B_SPLINE_CURVE_WITH_KNOTS ( 'NONE', 3,
 ( #785, #431, #4589, #2729 ),
 .UNSPECIFIED., .F., .F.,
 ( 4, 4 ),
 ( 0.004656695506220394354, 0.007337072593346776264 ),
 .UNSPECIFIED. ) ;
#5400 = EDGE_CURVE ( 'NONE', #708, #5408, #4004, .T. ) ;
#5401 = LINE ( 'NONE', #5344, #2362 ) ;
#5402 = VERTEX_POINT ( 'NONE', #3364 ) ;
#5403 = DIRECTION ( 'NONE',  ( -0.000000000000000000, 0.000000000000000000, 1.000000000000000000 ) ) ;
#5404 = DIRECTION ( 'NONE',  ( 0.000000000000000000, 0.000000000000000000, -1.000000000000000000 ) ) ;
#5405 = EDGE_CURVE ( 'NONE', #2028, #1825, #787, .T. ) ;
#5406 = CARTESIAN_POINT ( 'NONE',  ( 150.0000000000000284, 15.00000000000000000, -40.00000000000000711 ) ) ;
#5407 = EDGE_LOOP ( 'NONE', ( #4565, #5264, #276, #401 ) ) ;
#5408 = VERTEX_POINT ( 'NONE', #4892 ) ;
#5409 = LINE ( 'NONE', #3502, #1052 ) ;
#5410 = VERTEX_POINT ( 'NONE', #4822 ) ;
#5411 = CARTESIAN_POINT ( 'NONE',  ( -45.00000000000001421, 15.00000000000000000, 50.00000000000000000 ) ) ;
#5412 = LINE ( 'NONE', #4043, #5070 ) ;
#5413 = ORIENTED_EDGE ( 'NONE', *, *, #388, .F. ) ;
#5414 = CARTESIAN_POINT ( 'NONE',  ( 0.000000000000000000, -0.2499999999999998335, -1.312875263449798879 ) ) ;
#5415 = VERTEX_POINT ( 'NONE', #5241 ) ;
#5416 = AXIS2_PLACEMENT_3D ( 'NONE', #5775, #234, #649 ) ;
#5417 = DIRECTION ( 'NONE',  ( -0.000000000000000000, -0.000000000000000000, 1.000000000000000000 ) ) ;
#5418 = CARTESIAN_POINT ( 'NONE',  ( 62.50000000000001421, -1.951563910473909559E-15, 75.00000000000000000 ) ) ;
#5419 = LINE ( 'NONE', #3516, #4489 ) ;
#5420 = DIRECTION ( 'NONE',  ( -1.000000000000000000, 0.000000000000000000, 0.000000000000000000 ) ) ;
#5421 = ORIENTED_EDGE ( 'NONE', *, *, #130, .T. ) ;
#5422 = EDGE_CURVE ( 'NONE', #4352, #1680, #3885, .T. ) ;
#5423 =( NAMED_UNIT ( * ) PLANE_ANGLE_UNIT ( ) SI_UNIT ( $, .RADIAN. ) );
#5424 = DIRECTION ( 'NONE',  ( -1.000000000000000000, -0.000000000000000000, -0.000000000000000000 ) ) ;
#5425 = VECTOR ( 'NONE', #1534, 1000.000000000000000 ) ;
#5426 = EDGE_CURVE ( 'NONE', #2312, #2949, #4672, .T. ) ;
#5427 = ORIENTED_EDGE ( 'NONE', *, *, #3975, .T. ) ;
#5428 = DIRECTION ( 'NONE',  ( -1.000000000000000000, 0.000000000000000000, -0.000000000000000000 ) ) ;
#5429 = PRESENTATION_LAYER_ASSIGNMENT (  '', '', ( #4660 ) ) ;
#5430 = AXIS2_PLACEMENT_3D ( 'NONE', #2586, #5747, #5778 ) ;
#5431 = LINE ( 'NONE', #937, #4488 ) ;
#5432 = VECTOR ( 'NONE', #2178, 1000.000000000000000 ) ;
#5433 = AXIS2_PLACEMENT_3D ( 'NONE', #1743, #3598, #5728 ) ;
#5434 = CIRCLE ( 'NONE', #1364, 2.500000000000002220 ) ;
#5435 = DIRECTION ( 'NONE',  ( 1.000000000000000000, 0.000000000000000000, 0.000000000000000000 ) ) ;
#5436 = ADVANCED_BREP_SHAPE_REPRESENTATION ( '', ( #216, #5080 ), #4395 ) ;
#5437 = VERTEX_POINT ( 'NONE', #5211 ) ;
#5438 = EDGE_CURVE ( 'NONE', #4174, #1983, #1572, .T. ) ;
#5439 = ORIENTED_EDGE ( 'NONE', *, *, #1897, .T. ) ;
#5440 = VECTOR ( 'NONE', #4310, 1000.000000000000000 ) ;
#5441 = VECTOR ( 'NONE', #5004, 1000.000000000000000 ) ;
#5442 = CARTESIAN_POINT ( 'NONE',  ( 0.000000000000000000, 0.5149999999999917977, 2.350000000000000089 ) ) ;
#5443 = APPLICATION_CONTEXT ( 'automotive_design' ) ;
#5444 = ORIENTED_EDGE ( 'NONE', *, *, #3587, .T. ) ;
#5445 = CIRCLE ( 'NONE', #5926, 0.9999999999999991118 ) ;
#5446 = CARTESIAN_POINT ( 'NONE',  ( 150.0000000000000284, 15.00000000000000000, -49.99999999999998579 ) ) ;
#5447 = LINE ( 'NONE', #356, #5828 ) ;
#5448 = EDGE_LOOP ( 'NONE', ( #1713, #3150, #2241, #4361 ) ) ;
#5449 = DIRECTION ( 'NONE',  ( -1.000000000000000000, 0.000000000000000000, -0.000000000000000000 ) ) ;
#5450 = VERTEX_POINT ( 'NONE', #4793 ) ;
#5451 = ORIENTED_EDGE ( 'NONE', *, *, #1940, .F. ) ;
#5452 = VECTOR ( 'NONE', #309, 1000.000000000000000 ) ;
#5453 = CARTESIAN_POINT ( 'NONE',  ( 2.740000000000000213, 0.9838866223910001096, -0.5150000000000001243 ) ) ;
#5454 = DIRECTION ( 'NONE',  ( -0.000000000000000000, -0.000000000000000000, 1.000000000000000000 ) ) ;
#5455 = PRODUCT_DEFINITION_CONTEXT ( 'detailed design', #1797, 'design' ) ;
#5456 = DIRECTION ( 'NONE',  ( -1.000000000000000000, -0.000000000000000000, -0.000000000000000000 ) ) ;
#5457 =( GEOMETRIC_REPRESENTATION_CONTEXT ( 3 ) GLOBAL_UNCERTAINTY_ASSIGNED_CONTEXT ( ( #4346 ) ) GLOBAL_UNIT_ASSIGNED_CONTEXT ( ( #3816, #4644, #5577 ) ) REPRESENTATION_CONTEXT ( 'NONE', 'WORKASPACE' ) );
#5458 = LINE ( 'NONE', #4089, #5432 ) ;
#5459 = VERTEX_POINT ( 'NONE', #214 ) ;
#5460 = FACE_OUTER_BOUND ( 'NONE', #5015, .T. ) ;
#5461 = VECTOR ( 'NONE', #2696, 1000.000000000000000 ) ;
#5462 = EDGE_LOOP ( 'NONE', ( #2834, #2745, #2990, #175 ) ) ;
#5463 = FACE_BOUND ( 'NONE', #3874, .T. ) ;
#5464 = AXIS2_PLACEMENT_3D ( 'NONE', #3396, #2879, #1512 ) ;
#5465 = DIRECTION ( 'NONE',  ( 0.8571673013836870192, 0.000000000000000000, 0.5150380737757234151 ) ) ;
#5466 = ADVANCED_FACE ( 'NONE', ( #2016 ), #5693, .T. ) ;
#5467 = ADVANCED_FACE ( 'NONE', ( #3812 ), #3872, .T. ) ;
#5468 = DIRECTION ( 'NONE',  ( -1.000000000000000000, -0.000000000000000000, -0.000000000000000000 ) ) ;
#5469 = EDGE_LOOP ( 'NONE', ( #5658, #1995 ) ) ;
#5470 = ORIENTED_EDGE ( 'NONE', *, *, #4887, .T. ) ;
#5471 = ADVANCED_FACE ( 'NONE', ( #631 ), #601, .F. ) ;
#5472 = CARTESIAN_POINT ( 'NONE',  ( 75.00000000000001421, -15.00000000000000355, -75.00000000000000000 ) ) ;
#5473 = VECTOR ( 'NONE', #4409, 1000.000000000000000 ) ;
#5474 = ADVANCED_FACE ( 'NONE', ( #3423 ), #2970, .F. ) ;
#5475 = VERTEX_POINT ( 'NONE', #1136 ) ;
#5476 = LINE ( 'NONE', #1774, #2628 ) ;
#5477 = CIRCLE ( 'NONE', #1495, 10.00000000000000178 ) ;
#5478 = CARTESIAN_POINT ( 'NONE',  ( -45.00000000000001421, 50.00000000000000000, 45.00000000000000000 ) ) ;
#5479 = VERTEX_POINT ( 'NONE', #2500 ) ;
#5480 = CARTESIAN_POINT ( 'NONE',  ( 75.00000000000001421, 15.00000000000000000, 75.00000000000000000 ) ) ;
#5481 = VERTEX_POINT ( 'NONE', #3906 ) ;
#5482 = CARTESIAN_POINT ( 'NONE',  ( 67.00000000000000000, 0.000000000000000000, -9.500000000000000000 ) ) ;
#5483 = EDGE_CURVE ( 'NONE', #3078, #4039, #247, .T. ) ;
#5484 = CARTESIAN_POINT ( 'NONE',  ( 24.99999999999998224, 7.000000000000006217, -75.00000000000000000 ) ) ;
#5485 = DIRECTION ( 'NONE',  ( -0.000000000000000000, -1.000000000000000000, -0.000000000000000000 ) ) ;
#5486 = LINE ( 'NONE', #4522, #2533 ) ;
#5487 = VECTOR ( 'NONE', #4026, 1000.000000000000000 ) ;
#5488 = CARTESIAN_POINT ( 'NONE',  ( 75.00000000000001421, -15.00000000000000355, -75.00000000000000000 ) ) ;
#5489 = ORIENTED_EDGE ( 'NONE', *, *, #5762, .F. ) ;
#5490 = AXIS2_PLACEMENT_3D ( 'NONE', #1425, #4603, #1853 ) ;
#5491 = DIRECTION ( 'NONE',  ( -1.000000000000000000, -0.000000000000000000, -0.000000000000000000 ) ) ;
#5492 = AXIS2_PLACEMENT_3D ( 'NONE', #5549, #2637, #4499 ) ;
#5493 = ORIENTED_EDGE ( 'NONE', *, *, #4138, .T. ) ;
#5494 = CARTESIAN_POINT ( 'NONE',  ( 137.4999999999999716, -7.000000000000011546, 75.00000000000000000 ) ) ;
#5495 = DIRECTION ( 'NONE',  ( 0.000000000000000000, -1.000000000000000000, 0.000000000000000000 ) ) ;
#5496 = DIRECTION ( 'NONE',  ( 0.000000000000000000, 0.000000000000000000, 1.000000000000000000 ) ) ;
#5497 = ORIENTED_EDGE ( 'NONE', *, *, #159, .F. ) ;
#5498 = EDGE_CURVE ( 'NONE', #1875, #2650, #1600, .T. ) ;
#5499 = ORIENTED_EDGE ( 'NONE', *, *, #3942, .F. ) ;
#5500 = DIRECTION ( 'NONE',  ( 1.000000000000000000, -0.000000000000000000, -0.000000000000000000 ) ) ;
#5501 = EDGE_CURVE ( 'NONE', #2259, #3278, #5308, .T. ) ;
#5502 = CARTESIAN_POINT ( 'NONE',  ( 0.5000000000000000000, -0.2500000000000000000, 1.911797424705720116 ) ) ;
#5503 = ORIENTED_EDGE ( 'NONE', *, *, #1925, .T. ) ;
#5504 = ADVANCED_FACE ( 'NONE', ( #692 ), #4383, .F. ) ;
#5505 = FACE_OUTER_BOUND ( 'NONE', #5190, .T. ) ;
#5506 = CARTESIAN_POINT ( 'NONE',  ( 2.740000000000000213, 0.5150000000000035660, -0.9838866223905657904 ) ) ;
#5507 = VERTEX_POINT ( 'NONE', #3480 ) ;
#5508 = LINE ( 'NONE', #5964, #4866 ) ;
#5509 = ORIENTED_EDGE ( 'NONE', *, *, #1503, .F. ) ;
#5510 = DIRECTION ( 'NONE',  ( 0.000000000000000000, -1.000000000000000000, 0.000000000000000000 ) ) ;
#5511 = DIRECTION ( 'NONE',  ( 0.000000000000000000, 1.000000000000000000, 0.000000000000000000 ) ) ;
#5512 = CIRCLE ( 'NONE', #2108, 7.500000000000000000 ) ;
#5513 = DIRECTION ( 'NONE',  ( 1.000000000000000000, -0.000000000000000000, -0.000000000000000000 ) ) ;
#5514 = DIRECTION ( 'NONE',  ( -0.000000000000000000, 0.000000000000000000, -1.000000000000000000 ) ) ;
#5515 = DIRECTION ( 'NONE',  ( 0.000000000000000000, -0.000000000000000000, -1.000000000000000000 ) ) ;
#5516 = ORIENTED_EDGE ( 'NONE', *, *, #763, .T. ) ;
#5517 = EDGE_CURVE ( 'NONE', #4296, #2063, #4190, .T. ) ;
#5518 = FACE_OUTER_BOUND ( 'NONE', #72, .T. ) ;
#5519 = AXIS2_PLACEMENT_3D ( 'NONE', #1978, #3413, #5297 ) ;
#5520 = VERTEX_POINT ( 'NONE', #2569 ) ;
#5521 = LINE ( 'NONE', #820, #5452 ) ;
#5522 = CIRCLE ( 'NONE', #3203, 2.649999999999999467 ) ;
#5523 = DIRECTION ( 'NONE',  ( -1.000000000000000000, -0.000000000000000000, -0.000000000000000000 ) ) ;
#5524 = AXIS2_PLACEMENT_3D ( 'NONE', #2213, #3529, #3047 ) ;
#5525 = ORIENTED_EDGE ( 'NONE', *, *, #677, .F. ) ;
#5526 = VERTEX_POINT ( 'NONE', #5663 ) ;
#5527 = DIRECTION ( 'NONE',  ( 0.000000000000000000, 0.000000000000000000, 1.000000000000000000 ) ) ;
#5528 = VECTOR ( 'NONE', #339, 1000.000000000000000 ) ;
#5529 = CARTESIAN_POINT ( 'NONE',  ( 0.06760930072668894231, -0.9010842325122929708, -0.5150000000000000133 ) ) ;
#5530 = ORIENTED_EDGE ( 'NONE', *, *, #755, .T. ) ;
#5531 = CARTESIAN_POINT ( 'NONE',  ( -45.00000000000002842, 15.00000000000000000, -49.99999999999998579 ) ) ;
#5532 = CARTESIAN_POINT ( 'NONE',  ( 1.794155980045909482, 0.000000000000000000, 0.000000000000000000 ) ) ;
#5533 = AXIS2_PLACEMENT_3D ( 'NONE', #3908, #5724, #153 ) ;
#5534 = VERTEX_POINT ( 'NONE', #3840 ) ;
#5535 = ORIENTED_EDGE ( 'NONE', *, *, #2019, .T. ) ;
#5536 = SURFACE_STYLE_FILL_AREA ( #3243 ) ;
#5537 = PRODUCT_DEFINITION ( 'UNKNOWN', '', #5848, #2091 ) ;
#5538 = VECTOR ( 'NONE', #5273, 1000.000000000000000 ) ;
#5539 = VECTOR ( 'NONE', #19, 1000.000000000000000 ) ;
#5540 = CARTESIAN_POINT ( 'NONE',  ( -45.00000000000002842, 15.00000000000000000, -44.99999999999998579 ) ) ;
#5541 = CARTESIAN_POINT ( 'NONE',  ( 1.849560077140108172, -0.7556913915602447851, 0.5149999999999994582 ) ) ;
#5542 = EDGE_CURVE ( 'NONE', #111, #3568, #340, .T. ) ;
#5543 = FACE_OUTER_BOUND ( 'NONE', #4633, .T. ) ;
#5544 = LINE ( 'NONE', #4670, #705 ) ;
#5545 = ORIENTED_EDGE ( 'NONE', *, *, #1617, .F. ) ;
#5546 = VECTOR ( 'NONE', #5624, 1000.000000000000114 ) ;
#5547 = AXIS2_PLACEMENT_3D ( 'NONE', #757, #3405, #1910 ) ;
#5548 = CARTESIAN_POINT ( 'NONE',  ( 0.000000000000000000, 0.000000000000000000, 0.000000000000000000 ) ) ;
#5549 = CARTESIAN_POINT ( 'NONE',  ( 135.4999999999999716, 0.000000000000000000, 0.000000000000000000 ) ) ;
#5550 = AXIS2_PLACEMENT_3D ( 'NONE', #5442, #2520, #4872 ) ;
#5551 = STYLED_ITEM ( 'NONE', ( #2910 ), #5861 ) ;
#5552 = EDGE_CURVE ( 'NONE', #2883, #1725, #2177, .T. ) ;
#5553 = FACE_OUTER_BOUND ( 'NONE', #1018, .T. ) ;
#5554 = CYLINDRICAL_SURFACE ( 'NONE', #4162, 4.999999999999990230 ) ;
#5555 = FACE_OUTER_BOUND ( 'NONE', #3418, .T. ) ;
#5556 = VERTEX_POINT ( 'NONE', #4028 ) ;
#5557 = DIRECTION ( 'NONE',  ( -1.000000000000000000, 0.000000000000000000, 0.000000000000000000 ) ) ;
#5558 = SHAPE_DEFINITION_REPRESENTATION ( #3770, #2785 ) ;
#5559 = CARTESIAN_POINT ( 'NONE',  ( 67.00000000000000000, 0.000000000000000000, 9.500000000000000000 ) ) ;
#5560 = EDGE_LOOP ( 'NONE', ( #146, #5699, #77, #251 ) ) ;
#5561 = CARTESIAN_POINT ( 'NONE',  ( 77.00000000000001421, 1.469576158976823947E-15, -12.00000000000000000 ) ) ;
#5562 = ORIENTED_EDGE ( 'NONE', *, *, #3582, .T. ) ;
#5563 = ORIENTED_EDGE ( 'NONE', *, *, #3973, .T. ) ;
#5564 = DIRECTION ( 'NONE',  ( 0.000000000000000000, 0.000000000000000000, -1.000000000000000000 ) ) ;
#5565 = CARTESIAN_POINT ( 'NONE',  ( 24.99999999999998224, -7.000000000000006217, 65.00000000000000000 ) ) ;
#5566 = DIRECTION ( 'NONE',  ( 0.000000000000000000, 1.000000000000000000, 0.000000000000000000 ) ) ;
#5567 = DIRECTION ( 'NONE',  ( 1.000000000000000000, -0.000000000000000000, -0.000000000000000000 ) ) ;
#5568 = DIRECTION ( 'NONE',  ( 0.000000000000000000, 0.000000000000000000, 1.000000000000000000 ) ) ;
#5569 = ORIENTED_EDGE ( 'NONE', *, *, #131, .T. ) ;
#5570 = EDGE_CURVE ( 'NONE', #702, #4783, #1323, .T. ) ;
#5571 = ADVANCED_FACE ( 'NONE', ( #869 ), #1748, .T. ) ;
#5572 = DIRECTION ( 'NONE',  ( 0.000000000000000000, -0.000000000000000000, 1.000000000000000000 ) ) ;
#5573 = ADVANCED_FACE ( 'NONE', ( #2111, #2690 ), #5815, .F. ) ;
#5574 = EDGE_CURVE ( 'NONE', #3549, #2954, #5419, .T. ) ;
#5575 = DIRECTION ( 'NONE',  ( -1.000000000000000000, 0.000000000000000000, 0.000000000000000000 ) ) ;
#5576 = ORIENTED_EDGE ( 'NONE', *, *, #3208, .T. ) ;
#5577 =( NAMED_UNIT ( * ) SI_UNIT ( $, .STERADIAN. ) SOLID_ANGLE_UNIT ( ) );
#5578 = AXIS2_PLACEMENT_3D ( 'NONE', #4757, #4219, #5572 ) ;
#5579 = DIRECTION ( 'NONE',  ( 0.000000000000000000, -0.000000000000000000, 1.000000000000000000 ) ) ;
#5580 = ORIENTED_EDGE ( 'NONE', *, *, #159, .T. ) ;
#5581 = CARTESIAN_POINT ( 'NONE',  ( 67.00000000000000000, 0.000000000000000000, 8.500000000000000000 ) ) ;
#5582 = ADVANCED_FACE ( 'NONE', ( #3122 ), #4088, .T. ) ;
#5583 = DIRECTION ( 'NONE',  ( -1.000000000000000000, 0.000000000000000000, -0.000000000000000000 ) ) ;
#5584 = CARTESIAN_POINT ( 'NONE',  ( 137.4999999999999716, 6.999999999999985789, 75.00000000000001421 ) ) ;
#5585 = ORIENTED_EDGE ( 'NONE', *, *, #4323, .F. ) ;
#5586 = FACE_OUTER_BOUND ( 'NONE', #1652, .T. ) ;
#5587 = ORIENTED_EDGE ( 'NONE', *, *, #4293, .F. ) ;
#5588 = EDGE_LOOP ( 'NONE', ( #3668, #3005, #3000, #2972 ) ) ;
#5589 = DIRECTION ( 'NONE',  ( 1.000000000000000000, 0.000000000000000000, 0.000000000000000000 ) ) ;
#5590 = DIRECTION ( 'NONE',  ( 0.000000000000000000, 0.000000000000000000, 1.000000000000000000 ) ) ;
#5591 = CYLINDRICAL_SURFACE ( 'NONE', #1745, 12.00000000000000000 ) ;
#5592 = CARTESIAN_POINT ( 'NONE',  ( 77.00000000000001421, 0.000000000000000000, 9.500000000000000000 ) ) ;
#5593 = DIRECTION ( 'NONE',  ( 1.000000000000000000, 0.000000000000000000, 0.000000000000000000 ) ) ;
#5594 = ORIENTED_EDGE ( 'NONE', *, *, #994, .F. ) ;
#5595 = DIRECTION ( 'NONE',  ( 0.000000000000000000, 0.000000000000000000, 1.000000000000000000 ) ) ;
#5596 = DIRECTION ( 'NONE',  ( 0.000000000000000000, -1.224646799147352961E-16, 1.000000000000000000 ) ) ;
#5597 = PLANE ( 'NONE',  #5714 ) ;
#5598 = CARTESIAN_POINT ( 'NONE',  ( 24.99999999999998224, 7.000000000000006217, -75.00000000000000000 ) ) ;
#5599 = EDGE_CURVE ( 'NONE', #3406, #1699, #5732, .T. ) ;
#5600 = VECTOR ( 'NONE', #5317, 1000.000000000000000 ) ;
#5601 = ORIENTED_EDGE ( 'NONE', *, *, #673, .T. ) ;
#5602 =( LENGTH_UNIT ( ) NAMED_UNIT ( * ) SI_UNIT ( .MILLI., .METRE. ) );
#5603 = DIRECTION ( 'NONE',  ( 0.000000000000000000, -1.000000000000000000, 0.000000000000000000 ) ) ;
#5604 = EDGE_CURVE ( 'NONE', #2523, #1576, #33, .T. ) ;
#5605 = AXIS2_PLACEMENT_3D ( 'NONE', #4934, #414, #767 ) ;
#5606 = AXIS2_PLACEMENT_3D ( 'NONE', #4741, #4775, #1616 ) ;
#5607 = VERTEX_POINT ( 'NONE', #4920 ) ;
#5608 = CARTESIAN_POINT ( 'NONE',  ( 37.50000000000000711, 6.288372600415927295E-15, 75.00000000000000000 ) ) ;
#5609 = SHAPE_REPRESENTATION ( 'MAS-179', ( #3332, #1586, #3241, #5368, #43, #2943, #1093, #2265, #5750, #1392, #4502, #3904, #1961, #3806, #711, #4890, #4688, #1292, #4104, #1682, #338, #1871 ), #5085 ) ;
#5610 = DIRECTION ( 'NONE',  ( 0.000000000000000000, 0.000000000000000000, 1.000000000000000000 ) ) ;
#5611=STYLED_ITEM('',(#6027),#189);
#5612 = PRODUCT_DEFINITION_SHAPE ( 'NONE', 'NONE',  #5988 ) ;
#5613 = AXIS2_PLACEMENT_3D ( 'NONE', #884, #4001, #2499 ) ;
#5614 = CARTESIAN_POINT ( 'NONE',  ( -45.00000000000001421, 45.00000000000000000, 45.00000000000000000 ) ) ;
#5615 = EDGE_CURVE ( 'NONE', #2744, #3289, #3571, .T. ) ;
#5616 = CARTESIAN_POINT ( 'NONE',  ( 0.5477065543514070267, 0.000000000000000000, 0.000000000000000000 ) ) ;
#5617 = EDGE_LOOP ( 'NONE', ( #2824, #798, #465, #2877, #2434, #5665 ) ) ;
#5618 = VERTEX_POINT ( 'NONE', #749 ) ;
#5619 = LINE ( 'NONE', #3325, #1443 ) ;
#5620 = CARTESIAN_POINT ( 'NONE',  ( -36.33974596215562514, 45.00000000000000000, 44.99999999999999289 ) ) ;
#5621 = ORIENTED_EDGE ( 'NONE', *, *, #131, .F. ) ;
#5622 = CIRCLE ( 'NONE', #2332, 7.983406227920510467 ) ;
#5623 = CARTESIAN_POINT ( 'NONE',  ( 162.5000000000000000, 0.000000000000000000, -5.000000000000000000 ) ) ;
#5624 = DIRECTION ( 'NONE',  ( 0.8949343913984706411, 1.557891129246106293E-15, -0.4461977533473793778 ) ) ;
#5625 = FACE_OUTER_BOUND ( 'NONE', #4325, .T. ) ;
#5626 = ORIENTED_EDGE ( 'NONE', *, *, #2548, .F. ) ;
#5627 = VECTOR ( 'NONE', #3238, 1000.000000000000114 ) ;
#5628 = LINE ( 'NONE', #1475, #4135 ) ;
#5629 = APPLICATION_CONTEXT ( 'automotive_design' ) ;
#5630 = CARTESIAN_POINT ( 'NONE',  ( -45.00000000000001421, 40.00000000000000000, -45.00000000000000000 ) ) ;
#5631 = CIRCLE ( 'NONE', #983, 7.000000000000000000 ) ;
#5633 = AXIS2_PLACEMENT_3D ( 'NONE', #4008, #5856, #5161 ) ;
#5632 = DIRECTION ( 'NONE',  ( 0.000000000000000000, 0.000000000000000000, -1.000000000000000000 ) ) ;
#5634 = ORIENTED_EDGE ( 'NONE', *, *, #3505, .T. ) ;
#5635 = ORIENTED_EDGE ( 'NONE', *, *, #5132, .F. ) ;
#5636 = CARTESIAN_POINT ( 'NONE',  ( -45.00000000000001421, 40.00000000000000000, -50.00000000000000000 ) ) ;
#5637 = VECTOR ( 'NONE', #2884, 1000.000000000000000 ) ;
#5638 = ORIENTED_EDGE ( 'NONE', *, *, #1490, .F. ) ;
#5639 = DIRECTION ( 'NONE',  ( -1.000000000000000000, 3.469446951953614189E-16, 0.000000000000000000 ) ) ;
#5640 = EDGE_CURVE ( 'NONE', #1686, #5651, #4983, .T. ) ;
#5641 = PLANE ( 'NONE',  #2385 ) ;
#5642 = ITEM_DEFINED_TRANSFORMATION ( 'NONE', 'NONE', #1682,  #5080 ) ;
#5643 = EDGE_CURVE ( 'NONE', #1820, #3290, #814, .T. ) ;
#5644 = SURFACE_STYLE_FILL_AREA ( #5902 ) ;
#5645 = LINE ( 'NONE', #4534, #1546 ) ;
#5646 = SURFACE_STYLE_FILL_AREA ( #5824 ) ;
#5648 = ORIENTED_EDGE ( 'NONE', *, *, #3801, .F. ) ;
#5647 = EDGE_CURVE ( 'NONE', #5044, #60, #5486, .T. ) ;
#5649 = AXIS2_PLACEMENT_3D ( 'NONE', #964, #609, #5669 ) ;
#5650 = ORIENTED_EDGE ( 'NONE', *, *, #3322, .T. ) ;
#5651 = VERTEX_POINT ( 'NONE', #1487 ) ;
#5652 = SURFACE_STYLE_FILL_AREA ( #4781 ) ;
#5653 = AXIS2_PLACEMENT_3D ( 'NONE', #1904, #3308, #2366 ) ;
#5654 = DIRECTION ( 'NONE',  ( -0.8949343913984706411, 0.4461977533473793223, 0.000000000000000000 ) ) ;
#5655 = DIRECTION ( 'NONE',  ( -0.000000000000000000, -1.000000000000000000, -0.000000000000000000 ) ) ;
#5656 = DIRECTION ( 'NONE',  ( 0.000000000000000000, -0.000000000000000000, 1.000000000000000000 ) ) ;
#5657 = DIRECTION ( 'NONE',  ( 0.4461977533474923430, -0.8949343913984144638, 0.000000000000000000 ) ) ;
#5658 = ORIENTED_EDGE ( 'NONE', *, *, #5109, .T. ) ;
#5659 = DIRECTION ( 'NONE',  ( 1.000000000000000000, 0.000000000000000000, 0.000000000000000000 ) ) ;
#5660 = EDGE_CURVE ( 'NONE', #5157, #3394, #4495, .T. ) ;
#5661 = DIRECTION ( 'NONE',  ( 0.000000000000000000, 0.000000000000000000, -1.000000000000000000 ) ) ;
#5662 = FACE_OUTER_BOUND ( 'NONE', #2226, .T. ) ;
#5663 = CARTESIAN_POINT ( 'NONE',  ( 65.15000000000001990, -1.951563910473909559E-15, 65.00000000000000000 ) ) ;
#5664 = DIRECTION ( 'NONE',  ( 1.000000000000000000, -0.000000000000000000, 0.000000000000000000 ) ) ;
#5665 = ORIENTED_EDGE ( 'NONE', *, *, #2916, .F. ) ;
#5667 = ORIENTED_EDGE ( 'NONE', *, *, #5953, .T. ) ;
#5666 = PRODUCT_DEFINITION_SHAPE ( 'NONE', 'NONE',  #5978 ) ;
#5668 = SHAPE_REPRESENTATION_RELATIONSHIP ( 'NONE' , 'NONE' ,  #1113, #5861 ) ;
#5669 = DIRECTION ( 'NONE',  ( 0.000000000000000000, 0.000000000000000000, -1.000000000000000000 ) ) ;
#5670 = UNCERTAINTY_MEASURE_WITH_UNIT (LENGTH_MEASURE( 1.000000000000000082E-05 ), #4596, 'distance_accuracy_value', 'NONE');
#5671 = CARTESIAN_POINT ( 'NONE',  ( 25.00000000000000711, 7.000000000000011546, 65.00000000000000000 ) ) ;
#5672 = CARTESIAN_POINT ( 'NONE',  ( -49.33012701892221230, 45.00000000000000000, 52.49999999999999289 ) ) ;
#5673 = ITEM_DEFINED_TRANSFORMATION ( 'NONE', 'NONE', #1871,  #5080 ) ;
#5674 = DIRECTION ( 'NONE',  ( 0.000000000000000000, 0.000000000000000000, -1.000000000000000000 ) ) ;
#5675 = DIRECTION ( 'NONE',  ( 1.000000000000000000, 0.000000000000000000, 0.000000000000000000 ) ) ;
#5676 = ADVANCED_FACE ( 'NONE', ( #5850 ), #4458, .T. ) ;
#5677 = ORIENTED_EDGE ( 'NONE', *, *, #3978, .T. ) ;
#5678 = ADVANCED_FACE ( 'NONE', ( #2142 ), #5899, .T. ) ;
#5679 = VERTEX_POINT ( 'NONE', #2631 ) ;
#5680 = AXIS2_PLACEMENT_3D ( 'NONE', #2137, #4426, #4819 ) ;
#5681 = CARTESIAN_POINT ( 'NONE',  ( 196.6421356237309510, 6.123233995736766282E-16, -5.000000000000000000 ) ) ;
#5682 = EDGE_CURVE ( 'NONE', #5157, #3440, #5631, .T. ) ;
#5683 = LINE ( 'NONE', #4389, #4947 ) ;
#5684 = EDGE_LOOP ( 'NONE', ( #3426, #2559 ) ) ;
#5685 = CARTESIAN_POINT ( 'NONE',  ( 35.00000000000000000, 6.288372600415927295E-15, -65.00000000000000000 ) ) ;
#5686 = LINE ( 'NONE', #1527, #1754 ) ;
#5687 = FACE_OUTER_BOUND ( 'NONE', #1818, .T. ) ;
#5688 = ORIENTED_EDGE ( 'NONE', *, *, #5105, .T. ) ;
#5689 = APPLICATION_PROTOCOL_DEFINITION ( 'draft international standard', 'automotive_design', 1998, #2962 ) ;
#5690 = CARTESIAN_POINT ( 'NONE',  ( -45.00000000000001421, 50.00000000000000000, 45.00000000000000000 ) ) ;
#5691 = FACE_OUTER_BOUND ( 'NONE', #5696, .T. ) ;
#5692 = DIRECTION ( 'NONE',  ( 0.000000000000000000, 0.000000000000000000, 1.000000000000000000 ) ) ;
#5693 = CYLINDRICAL_SURFACE ( 'NONE', #3786, 2.500000000000000000 ) ;
#5694 = DIRECTION ( 'NONE',  ( 0.000000000000000000, 0.000000000000000000, 1.000000000000000000 ) ) ;
#5695 = ADVANCED_FACE ( 'NONE', ( #4637 ), #1351, .F. ) ;
#5696 = EDGE_LOOP ( 'NONE', ( #274, #240 ) ) ;
#5697 = EDGE_LOOP ( 'NONE', ( #5223, #2703 ) ) ;
#5698 = CARTESIAN_POINT ( 'NONE',  ( 75.00000000000001421, 15.00000000000000000, 75.00000000000000000 ) ) ;
#5699 = ORIENTED_EDGE ( 'NONE', *, *, #2535, .T. ) ;
#5700 = CARTESIAN_POINT ( 'NONE',  ( 0.000000000000000000, 0.000000000000000000, 0.000000000000000000 ) ) ;
#5701 = VECTOR ( 'NONE', #1466, 1000.000000000000000 ) ;
#5702 = LINE ( 'NONE', #1548, #2480 ) ;
#5703 = CARTESIAN_POINT ( 'NONE',  ( 162.4999999999999716, 6.999999999999985789, 65.00000000000000000 ) ) ;
#5704 = AXIS2_PLACEMENT_3D ( 'NONE', #197, #5325, #1522 ) ;
#5705 = ORIENTED_EDGE ( 'NONE', *, *, #2180, .F. ) ;
#5706 = ORIENTED_EDGE ( 'NONE', *, *, #97, .T. ) ;
#5707 = PLANE ( 'NONE',  #4067 ) ;
#5708 = LINE ( 'NONE', #1591, #386 ) ;
#5709 = ORIENTED_EDGE ( 'NONE', *, *, #5949, .T. ) ;
#5710 = DIRECTION ( 'NONE',  ( 1.000000000000000000, -0.000000000000000000, -0.000000000000000000 ) ) ;
#5711 = LINE ( 'NONE', #4302, #1273 ) ;
#5712 = AXIS2_PLACEMENT_3D ( 'NONE', #2072, #4447, #3983 ) ;
#5713 = CYLINDRICAL_SURFACE ( 'NONE', #3504, 10.00000000000000178 ) ;
#5714 = AXIS2_PLACEMENT_3D ( 'NONE', #3777, #1441, #5496 ) ;
#5715 = ORIENTED_EDGE ( 'NONE', *, *, #1940, .T. ) ;
#5716 = APPLICATION_PROTOCOL_DEFINITION ( 'draft international standard', 'automotive_design', 1998, #5443 ) ;
#5717 = DIRECTION ( 'NONE',  ( 0.000000000000000000, 0.000000000000000000, 1.000000000000000000 ) ) ;
#5718 = AXIS2_PLACEMENT_3D ( 'NONE', #4946, #2666, #1264 ) ;
#5719 = ADVANCED_FACE ( 'NONE', ( #1809 ), #451, .F. ) ;
#5720 = FACE_OUTER_BOUND ( 'NONE', #187, .T. ) ;
#5721 = CARTESIAN_POINT ( 'NONE',  ( 2.740000000000000213, -0.5150000000000022338, 0.6774776749089210792 ) ) ;
#5722 = ADVANCED_BREP_SHAPE_REPRESENTATION ( '', ( #4206, #5080 ), #3707 ) ;
#5723 = CARTESIAN_POINT ( 'NONE',  ( -45.00000000000001421, 50.00000000000000000, 45.00000000000000000 ) ) ;
#5724 = DIRECTION ( 'NONE',  ( -1.000000000000000000, -0.000000000000000000, -0.000000000000000000 ) ) ;
#5725 = ORIENTED_EDGE ( 'NONE', *, *, #677, .T. ) ;
#5726 = CIRCLE ( 'NONE', #887, 7.864440107515430434 ) ;
#5727 = VECTOR ( 'NONE', #593, 1000.000000000000000 ) ;
#5728 = DIRECTION ( 'NONE',  ( 0.000000000000000000, 0.000000000000000000, -1.000000000000000000 ) ) ;
#5729 = SURFACE_STYLE_USAGE ( .BOTH. , #1140 ) ;
#5730 = CARTESIAN_POINT ( 'NONE',  ( 77.00000000000001421, 0.000000000000000000, 12.00000000000000000 ) ) ;
#5731 = EDGE_CURVE ( 'NONE', #554, #5930, #5445, .T. ) ;
#5732 = CIRCLE ( 'NONE', #3125, 5.000000000000004441 ) ;
#5733 = CIRCLE ( 'NONE', #1368, 5.000000000000004441 ) ;
#5734 = EDGE_LOOP ( 'NONE', ( #1544, #4069, #1066, #4808 ) ) ;
#5735 = AXIS2_PLACEMENT_3D ( 'NONE', #3731, #4224, #5579 ) ;
#5736 = MECHANICAL_DESIGN_GEOMETRIC_PRESENTATION_REPRESENTATION (  '', ( #984 ), #1575 ) ;
#5737 = DIRECTION ( 'NONE',  ( 0.000000000000000000, 0.000000000000000000, 1.000000000000000000 ) ) ;
#5738 = EDGE_CURVE ( 'NONE', #4020, #1770, #1385, .T. ) ;
#5739 = DIRECTION ( 'NONE',  ( 1.000000000000000000, 0.000000000000000000, 0.000000000000000000 ) ) ;
#5740 =( GEOMETRIC_REPRESENTATION_CONTEXT ( 3 ) GLOBAL_UNCERTAINTY_ASSIGNED_CONTEXT ( ( #4494 ) ) GLOBAL_UNIT_ASSIGNED_CONTEXT ( ( #4587, #5423, #4056 ) ) REPRESENTATION_CONTEXT ( 'NONE', 'WORKASPACE' ) );
#5741 = ORIENTED_EDGE ( 'NONE', *, *, #3702, .F. ) ;
#5742 = VERTEX_POINT ( 'NONE', #4182 ) ;
#5743 = FILL_AREA_STYLE_COLOUR ( '', #11 ) ;
#5744 = PRODUCT_DEFINITION_FORMATION_WITH_SPECIFIED_SOURCE ( 'ANY', '', #1635, .NOT_KNOWN. ) ;
#5745 = CARTESIAN_POINT ( 'NONE',  ( 75.00000000000001421, 1.347111479062087764E-16, 10.59999999999999787 ) ) ;
#5746 = ORIENTED_EDGE ( 'NONE', *, *, #3826, .T. ) ;
#5747 = DIRECTION ( 'NONE',  ( 1.000000000000000000, 0.000000000000000000, 0.000000000000000000 ) ) ;
#5748 = DIRECTION ( 'NONE',  ( -0.000000000000000000, -0.000000000000000000, 1.000000000000000000 ) ) ;
#5749 = PRODUCT_DEFINITION_SHAPE ( 'NONE', 'NONE',  #3543 ) ;
#5750 = AXIS2_PLACEMENT_3D ( 'NONE', #2299, #4154, #5183 ) ;
#5751 = APPLICATION_CONTEXT ( 'automotive_design' ) ;
#5752 = CARTESIAN_POINT ( 'NONE',  ( 40.00000000000000711, 6.594534300202765954E-15, -65.00000000000000000 ) ) ;
#5753 = ORIENTED_EDGE ( 'NONE', *, *, #5072, .F. ) ;
#5754 = DIRECTION ( 'NONE',  ( 1.000000000000000000, 0.000000000000000000, 0.000000000000000000 ) ) ;
#5755 = CARTESIAN_POINT ( 'NONE',  ( 0.9586399445693768451, 0.5149999999999971267, 0.8293189044373084906 ) ) ;
#5756 = CARTESIAN_POINT ( 'NONE',  ( 162.5000000000000000, 0.000000000000000000, 0.000000000000000000 ) ) ;
#5757 = CARTESIAN_POINT ( 'NONE',  ( 0.000000000000000000, 0.5150000000000083400, -2.349999999999997424 ) ) ;
#5758 = LINE ( 'NONE', #3518, #5346 ) ;
#5759 = ADVANCED_FACE ( 'NONE', ( #2809, #927 ), #2, .T. ) ;
#5760 = ORIENTED_EDGE ( 'NONE', *, *, #4434, .T. ) ;
#5761 = EDGE_CURVE ( 'NONE', #2555, #1563, #2839, .T. ) ;
#5762 = EDGE_CURVE ( 'NONE', #1033, #5742, #3331, .T. ) ;
#5763 = ORIENTED_EDGE ( 'NONE', *, *, #3818, .F. ) ;
#5764 = LINE ( 'NONE', #2090, #5185 ) ;
#5765 = ADVANCED_FACE ( 'NONE', ( #3692 ), #2354, .F. ) ;
#5766 = ORIENTED_EDGE ( 'NONE', *, *, #4249, .F. ) ;
#5767 =( NAMED_UNIT ( * ) PLANE_ANGLE_UNIT ( ) SI_UNIT ( $, .RADIAN. ) );
#5768 = CARTESIAN_POINT ( 'NONE',  ( 67.00000000000000000, 1.224646799147354440E-16, 10.49999999999999822 ) ) ;
#5769 = PRODUCT_DEFINITION_SHAPE ( 'NONE', 'NONE',  #5980 ) ;
#5770 = CYLINDRICAL_SURFACE ( 'NONE', #5225, 7.500000000000000000 ) ;
#5771 = ORIENTED_EDGE ( 'NONE', *, *, #1120, .F. ) ;
#5772 = ADVANCED_FACE ( 'NONE', ( #5543 ), #1434, .T. ) ;
#5773 = ORIENTED_EDGE ( 'NONE', *, *, #4694, .T. ) ;
#5774 = DIRECTION ( 'NONE',  ( 1.007709689656716815E-16, 1.000000000000000000, 3.606821995490527259E-15 ) ) ;
#5775 = CARTESIAN_POINT ( 'NONE',  ( -45.00000000000001421, 30.00000000000000355, 45.00000000000000000 ) ) ;
#5776 = ORIENTED_EDGE ( 'NONE', *, *, #2693, .T. ) ;
#5777 = AXIS2_PLACEMENT_3D ( 'NONE', #4740, #4350, #579 ) ;
#5778 = DIRECTION ( 'NONE',  ( 0.000000000000000000, 0.000000000000000000, -1.000000000000000000 ) ) ;
#5779 = DIRECTION ( 'NONE',  ( 0.000000000000000000, -0.000000000000000000, -1.000000000000000000 ) ) ;
#5780 = DIRECTION ( 'NONE',  ( 1.000000000000000000, 0.000000000000000000, 0.000000000000000000 ) ) ;
#5781 = AXIS2_PLACEMENT_3D ( 'NONE', #2107, #687, #3058 ) ;
#5782 = ORIENTED_EDGE ( 'NONE', *, *, #4602, .F. ) ;
#5783 =( LENGTH_UNIT ( ) NAMED_UNIT ( * ) SI_UNIT ( .MILLI., .METRE. ) );
#5784 = CARTESIAN_POINT ( 'NONE',  ( 2.740000000000000213, -0.5150000000000034550, 0.9838866223909983333 ) ) ;
#5785 = DIRECTION ( 'NONE',  ( -0.5000000000000004441, 0.000000000000000000, -0.8660254037844383745 ) ) ;
#5786 = DIRECTION ( 'NONE',  ( 0.000000000000000000, 0.000000000000000000, -1.000000000000000000 ) ) ;
#5787 = DIRECTION ( 'NONE',  ( 0.4999999999999993894, 0.000000000000000000, -0.8660254037844389297 ) ) ;
#5788 = DIRECTION ( 'NONE',  ( -0.000000000000000000, -0.000000000000000000, -1.000000000000000000 ) ) ;
#5789 = ORIENTED_EDGE ( 'NONE', *, *, #458, .T. ) ;
#5790 = EDGE_LOOP ( 'NONE', ( #4198, #4592, #4347, #2144, #1404 ) ) ;
#5791 = CARTESIAN_POINT ( 'NONE',  ( -49.33012701892221230, 45.00000000000000000, 37.50000000000000000 ) ) ;
#5792 = PRODUCT_DEFINITION_CONTEXT ( 'detailed design', #3579, 'design' ) ;
#5793 = VERTEX_POINT ( 'NONE', #30 ) ;
#5794 = ADVANCED_FACE ( 'NONE', ( #5155 ), #2722, .T. ) ;
#5795 = EDGE_CURVE ( 'NONE', #4352, #771, #987, .T. ) ;
#5796 = LINE ( 'NONE', #1243, #1815 ) ;
#5797 = AXIS2_PLACEMENT_3D ( 'NONE', #3215, #1349, #2229 ) ;
#5798 = LINE ( 'NONE', #4930, #3877 ) ;
#5799 = ORIENTED_EDGE ( 'NONE', *, *, #1751, .T. ) ;
#5800 = ORIENTED_EDGE ( 'NONE', *, *, #4621, .T. ) ;
#5801 = DIRECTION ( 'NONE',  ( -0.000000000000000000, -1.000000000000000000, -0.000000000000000000 ) ) ;
#5802 = AXIS2_PLACEMENT_3D ( 'NONE', #5453, #5966, #3661 ) ;
#5803 = EDGE_CURVE ( 'NONE', #5946, #764, #3769, .T. ) ;
#5804 = DIRECTION ( 'NONE',  ( -0.000000000000000000, 0.000000000000000000, 1.000000000000000000 ) ) ;
#5805 = ORIENTED_EDGE ( 'NONE', *, *, #2239, .F. ) ;
#5806 = FACE_OUTER_BOUND ( 'NONE', #1377, .T. ) ;
#5807 = CYLINDRICAL_SURFACE ( 'NONE', #3126, 5.000000000000004441 ) ;
#5808 = CARTESIAN_POINT ( 'NONE',  ( 0.000000000000000000, 0.2499999999999982792, 2.000000000000001776 ) ) ;
#5809 = ORIENTED_EDGE ( 'NONE', *, *, #3791, .F. ) ;
#5810 = AXIS2_PLACEMENT_3D ( 'NONE', #1058, #616, #2485 ) ;
#5811 = DIRECTION ( 'NONE',  ( 0.000000000000000000, 1.000000000000000000, 0.000000000000000000 ) ) ;
#5812 = DIRECTION ( 'NONE',  ( 0.000000000000000000, 1.000000000000000000, 0.000000000000000000 ) ) ;
#5813 = AXIS2_PLACEMENT_3D ( 'NONE', #5630, #3303, #996 ) ;
#5814 = CARTESIAN_POINT ( 'NONE',  ( 3.016506661494197328, 7.007546303702493782E-17, 0.000000000000000000 ) ) ;
#5815 = PLANE ( 'NONE',  #2640 ) ;
#5816 = DIRECTION ( 'NONE',  ( 0.000000000000000000, -3.606821995490527259E-15, 1.000000000000000000 ) ) ;
#5817 = EDGE_LOOP ( 'NONE', ( #3919, #3255, #1798, #756 ) ) ;
#5818 = APPLICATION_PROTOCOL_DEFINITION ( 'draft international standard', 'automotive_design', 1998, #2734 ) ;
#5819 = AXIS2_PLACEMENT_3D ( 'NONE', #4944, #3570, #1781 ) ;
#5820 = CARTESIAN_POINT ( 'NONE',  ( 75.00000000000001421, -7.000000000000006217, -65.00000000000000000 ) ) ;
#5821 = B_SPLINE_CURVE_WITH_KNOTS ( 'NONE', 3,
 ( #2025, #665, #2181, #3667 ),
 .UNSPECIFIED., .F., .F.,
 ( 4, 4 ),
 ( 0.004656695504653254707, 0.007337072591785142629 ),
 .UNSPECIFIED. ) ;
#5822 = ORIENTED_EDGE ( 'NONE', *, *, #1723, .T. ) ;
#5823 = AXIS2_PLACEMENT_3D ( 'NONE', #1324, #366, #3089 ) ;
#5824 = FILL_AREA_STYLE ('',( #2858 ) ) ;
#5825 = DIRECTION ( 'NONE',  ( -0.000000000000000000, -0.000000000000000000, 1.000000000000000000 ) ) ;
#5826 = AXIS2_PLACEMENT_3D ( 'NONE', #2613, #5801, #4478 ) ;
#5827 = VECTOR ( 'NONE', #2134, 1000.000000000000000 ) ;
#5828 = VECTOR ( 'NONE', #1194, 1000.000000000000000 ) ;
#5829 = DIRECTION ( 'NONE',  ( 0.000000000000000000, 0.000000000000000000, -1.000000000000000000 ) ) ;
#5830 = TOROIDAL_SURFACE ( 'NONE', #1671, 1.336466033005844434, 0.5999999999999999778 ) ;
#5831 = VERTEX_POINT ( 'NONE', #4123 ) ;
#5832 = CIRCLE ( 'NONE', #5633, 5.499999999999991118 ) ;
#5833 = ADVANCED_FACE ( 'NONE', ( #1916 ), #4580, .F. ) ;
#5834 = ORIENTED_EDGE ( 'NONE', *, *, #1082, .F. ) ;
#5835 = EDGE_CURVE ( 'NONE', #5354, #1426, #1464, .T. ) ;
#5836 = FACE_OUTER_BOUND ( 'NONE', #4090, .T. ) ;
#5837 =( GEOMETRIC_REPRESENTATION_CONTEXT ( 3 ) GLOBAL_UNCERTAINTY_ASSIGNED_CONTEXT ( ( #2947 ) ) GLOBAL_UNIT_ASSIGNED_CONTEXT ( ( #880, #3616, #2736 ) ) REPRESENTATION_CONTEXT ( 'NONE', 'WORKASPACE' ) );
#5838 = VERTEX_POINT ( 'NONE', #903 ) ;
#5839 = ADVANCED_FACE ( 'NONE', ( #4316 ), #5830, .T. ) ;
#5840 = DIRECTION ( 'NONE',  ( 0.000000000000000000, 0.000000000000000000, 1.000000000000000000 ) ) ;
#5841 = CARTESIAN_POINT ( 'NONE',  ( 37.50000000000000711, 6.288372600415927295E-15, 65.00000000000000000 ) ) ;
#5842 = ORIENTED_EDGE ( 'NONE', *, *, #3902, .T. ) ;
#5843 = CARTESIAN_POINT ( 'NONE',  ( 77.00000000000001421, 1.469576158976823947E-15, -12.00000000000000000 ) ) ;
#5844 = ORIENTED_EDGE ( 'NONE', *, *, #4877, .F. ) ;
#5845 =( GEOMETRIC_REPRESENTATION_CONTEXT ( 3 ) GLOBAL_UNCERTAINTY_ASSIGNED_CONTEXT ( ( #779 ) ) GLOBAL_UNIT_ASSIGNED_CONTEXT ( ( #1753, #4462, #3574 ) ) REPRESENTATION_CONTEXT ( 'NONE', 'WORKASPACE' ) );
#5846 = LINE ( 'NONE', #267, #456 ) ;
#5847 = DIRECTION ( 'NONE',  ( 0.000000000000000000, 0.000000000000000000, 1.000000000000000000 ) ) ;
#5848 = PRODUCT_DEFINITION_FORMATION_WITH_SPECIFIED_SOURCE ( 'ANY', '', #58, .NOT_KNOWN. ) ;
#5849 = DIRECTION ( 'NONE',  ( 0.000000000000000000, 0.000000000000000000, 1.000000000000000000 ) ) ;
#5850 = FACE_OUTER_BOUND ( 'NONE', #4661, .T. ) ;
#5851 = CARTESIAN_POINT ( 'NONE',  ( -45.00000000000002842, 15.00000000000000000, -44.99999999999998579 ) ) ;
#5852 = ORIENTED_EDGE ( 'NONE', *, *, #4514, .T. ) ;
#5853 = ADVANCED_FACE ( 'NONE', ( #1514 ), #4584, .F. ) ;
#5854 = PLANE ( 'NONE',  #5274 ) ;
#5855 = VERTEX_POINT ( 'NONE', #2336 ) ;
#5856 = DIRECTION ( 'NONE',  ( -0.000000000000000000, -0.000000000000000000, 1.000000000000000000 ) ) ;
#5857 = DIRECTION ( 'NONE',  ( 0.000000000000000000, 0.000000000000000000, -1.000000000000000000 ) ) ;
#5858 = LINE ( 'NONE', #5380, #5142 ) ;
#5859 = ORIENTED_EDGE ( 'NONE', *, *, #1503, .T. ) ;
#5860 = ORIENTED_EDGE ( 'NONE', *, *, #2976, .T. ) ;
#5861 = ADVANCED_BREP_SHAPE_REPRESENTATION ( '', ( #2182, #5080 ), #4776 ) ;
#5862 = DIRECTION ( 'NONE',  ( -0.000000000000000000, -1.000000000000000000, -0.000000000000000000 ) ) ;
#5863 = ORIENTED_EDGE ( 'NONE', *, *, #1306, .F. ) ;
#5864 = FACE_OUTER_BOUND ( 'NONE', #4175, .T. ) ;
#5865 = CARTESIAN_POINT ( 'NONE',  ( 67.00000000000001421, 8.572527594031473190E-16, 7.000000000000000000 ) ) ;
#5866 = ADVANCED_FACE ( 'NONE', ( #5217 ), #5353, .T. ) ;
#5867 = ORIENTED_EDGE ( 'NONE', *, *, #3145, .T. ) ;
#5868 = DIRECTION ( 'NONE',  ( 0.000000000000000000, 0.000000000000000000, 1.000000000000000000 ) ) ;
#5869 = ORIENTED_EDGE ( 'NONE', *, *, #1756, .F. ) ;
#5870 = ADVANCED_FACE ( 'NONE', ( #4199 ), #520, .F. ) ;
#5871 = CARTESIAN_POINT ( 'NONE',  ( 2.740000000000000213, 0.5149999999999965716, 0.9838866223910015529 ) ) ;
#5872 = CARTESIAN_POINT ( 'NONE',  ( 77.00000000000001421, 0.000000000000000000, 9.500000000000000000 ) ) ;
#5873 = UNCERTAINTY_MEASURE_WITH_UNIT (LENGTH_MEASURE( 1.000000000000000082E-05 ), #2695, 'distance_accuracy_value', 'NONE');
#5874 = CARTESIAN_POINT ( 'NONE',  ( -45.00000000000001421, 40.00000000000000000, 39.99999999999999289 ) ) ;
#5875 = CYLINDRICAL_SURFACE ( 'NONE', #1457, 2.500000000000002220 ) ;
#5876 = ORIENTED_EDGE ( 'NONE', *, *, #3942, .T. ) ;
#5877 = CIRCLE ( 'NONE', #71, 2.649999999999999467 ) ;
#5878 = CARTESIAN_POINT ( 'NONE',  ( 67.00000000000001421, 0.000000000000000000, 0.000000000000000000 ) ) ;
#5879 = EDGE_CURVE ( 'NONE', #764, #1436, #1945, .T. ) ;
#5880 = ADVANCED_FACE ( 'NONE', ( #5136 ), #4651, .F. ) ;
#5881 = VERTEX_POINT ( 'NONE', #1454 ) ;
#5882 = SHAPE_REPRESENTATION ( 'movable block', ( #5080 ), #5457 ) ;
#5883 = PLANE ( 'NONE',  #5927 ) ;
#5884 = APPLICATION_PROTOCOL_DEFINITION ( 'draft international standard', 'automotive_design', 1998, #5629 ) ;
#5885 = CARTESIAN_POINT ( 'NONE',  ( 0.06760930072668894231, 0.9010842325122832008, -0.5150000000000000133 ) ) ;
#5886 = CARTESIAN_POINT ( 'NONE',  ( 0.000000000000000000, 45.00000000000000000, 0.000000000000000000 ) ) ;
#5887 = ORIENTED_EDGE ( 'NONE', *, *, #4432, .F. ) ;
#5888 = ORIENTED_EDGE ( 'NONE', *, *, #2488, .T. ) ;
#5889 = ORIENTED_EDGE ( 'NONE', *, *, #565, .T. ) ;
#5890 = CARTESIAN_POINT ( 'NONE',  ( -74.99999999999998579, -15.00000000000000000, 75.00000000000000000 ) ) ;
#5891 = CYLINDRICAL_SURFACE ( 'NONE', #1852, 4.999999999999990230 ) ;
#5892 = ORIENTED_EDGE ( 'NONE', *, *, #496, .F. ) ;
#5893 = CARTESIAN_POINT ( 'NONE',  ( 8.000000000000000000, -4.896755294805453861E-15, 0.5150000000000000133 ) ) ;
#5894 = ORIENTED_EDGE ( 'NONE', *, *, #3582, .F. ) ;
#5895 = ORIENTED_EDGE ( 'NONE', *, *, #2791, .F. ) ;
#5896 = VECTOR ( 'NONE', #504, 1000.000000000000000 ) ;
#5897 = CARTESIAN_POINT ( 'NONE',  ( -45.00000000000001421, 15.00000000000000000, 39.99999999999999289 ) ) ;
#5898 = LINE ( 'NONE', #1746, #5528 ) ;
#5899 = CYLINDRICAL_SURFACE ( 'NONE', #2149, 5.000000000000000000 ) ;
#5900 = CARTESIAN_POINT ( 'NONE',  ( 62.50000000000001421, -1.951563910473909559E-15, -65.00000000000000000 ) ) ;
#5901 = ORIENTED_EDGE ( 'NONE', *, *, #3755, .T. ) ;
#5902 = FILL_AREA_STYLE ('',( #783 ) ) ;
#5903 = EDGE_CURVE ( 'NONE', #1334, #3605, #123, .T. ) ;
#5904 = CARTESIAN_POINT ( 'NONE',  ( 55.00000000000000711, 0.000000000000000000, 0.000000000000000000 ) ) ;
#5905 = VECTOR ( 'NONE', #4147, 1000.000000000000000 ) ;
#5906 = AXIS2_PLACEMENT_3D ( 'NONE', #3931, #1692, #5786 ) ;
#5907 = ORIENTED_EDGE ( 'NONE', *, *, #1010, .F. ) ;
#5908 = EDGE_CURVE ( 'NONE', #605, #3368, #3796, .T. ) ;
#5909 = CARTESIAN_POINT ( 'NONE',  ( 172.5000000000000284, 6.123233995736766282E-16, -5.000000000000000000 ) ) ;
#5910 = CIRCLE ( 'NONE', #1159, 10.00000000000000178 ) ;
#5911 = CIRCLE ( 'NONE', #3399, 2.500000000000002220 ) ;
#5912 = EDGE_CURVE ( 'NONE', #1699, #2678, #5167, .T. ) ;
#5913 = LINE ( 'NONE', #3257, #2994 ) ;
#5914 = VECTOR ( 'NONE', #603, 1000.000000000000000 ) ;
#5915 = CIRCLE ( 'NONE', #3306, 5.000000000000004441 ) ;
#5916 = DIRECTION ( 'NONE',  ( 0.8949343913984706411, -0.4461977533473793778, 0.000000000000000000 ) ) ;
#5917 = EDGE_LOOP ( 'NONE', ( #5033, #1689, #350, #1302 ) ) ;
#5918 = ORIENTED_EDGE ( 'NONE', *, *, #1723, .F. ) ;
#5919 = AXIS2_PLACEMENT_3D ( 'NONE', #743, #3567, #3181 ) ;
#5920 = AXIS2_PLACEMENT_3D ( 'NONE', #5841, #1710, #5387 ) ;
#5921 = EDGE_CURVE ( 'NONE', #3435, #4171, #4773, .T. ) ;
#5922 = DIRECTION ( 'NONE',  ( 1.000000000000000000, 0.000000000000000000, 0.000000000000000000 ) ) ;
#5923 = PRESENTATION_STYLE_ASSIGNMENT (( #3984 ) ) ;
#5924 = MECHANICAL_DESIGN_GEOMETRIC_PRESENTATION_REPRESENTATION (  '', ( #2639 ), #989 ) ;
#5925 = EDGE_LOOP ( 'NONE', ( #1257, #3803, #2033, #5135 ) ) ;
#5926 = AXIS2_PLACEMENT_3D ( 'NONE', #2296, #5567, #1836 ) ;
#5927 = AXIS2_PLACEMENT_3D ( 'NONE', #2763, #2643, #4594 ) ;
#5928 = FACE_OUTER_BOUND ( 'NONE', #735, .T. ) ;
#5929 = CARTESIAN_POINT ( 'NONE',  ( 2.740000000000000213, 0.000000000000000000, 0.000000000000000000 ) ) ;
#5930 = VERTEX_POINT ( 'NONE', #5581 ) ;
#5931 = CARTESIAN_POINT ( 'NONE',  ( 35.00000000000000000, 6.288372600415927295E-15, -65.00000000000000000 ) ) ;
#5932 = ORIENTED_EDGE ( 'NONE', *, *, #4293, .T. ) ;
#5933 = DIRECTION ( 'NONE',  ( 1.000000000000000000, 0.000000000000000000, 0.000000000000000000 ) ) ;
#5934 = VECTOR ( 'NONE', #2541, 1000.000000000000114 ) ;
#5935 = CARTESIAN_POINT ( 'NONE',  ( 137.4999999999999716, 0.000000000000000000, -5.000000000000000000 ) ) ;
#5936 = FACE_OUTER_BOUND ( 'NONE', #422, .T. ) ;
#5937 = PRODUCT_DEFINITION_CONTEXT ( 'detailed design', #4943, 'design' ) ;
#5938 = CARTESIAN_POINT ( 'NONE',  ( -45.00000000000001421, 15.00000000000000000, 45.00000000000000000 ) ) ;
#5939 = COLOUR_RGB ( '',0.8941176470588234615, 0.8941176470588234615, 0.8941176470588234615 ) ;
#5940 = DIRECTION ( 'NONE',  ( -0.000000000000000000, -0.000000000000000000, -1.000000000000000000 ) ) ;
#5941 = ORIENTED_EDGE ( 'NONE', *, *, #4810, .T. ) ;
#5942 =( NAMED_UNIT ( * ) SI_UNIT ( $, .STERADIAN. ) SOLID_ANGLE_UNIT ( ) );
#5943 = CARTESIAN_POINT ( 'NONE',  ( 59.85000000000001563, -1.627032508699861061E-15, 65.00000000000000000 ) ) ;
#5944 = AXIS2_PLACEMENT_3D ( 'NONE', #2325, #3726, #3746 ) ;
#5945 = CONICAL_SURFACE ( 'NONE', #5284, 3077.683537175319998, 1.256637061435923686 ) ;
#5946 = VERTEX_POINT ( 'NONE', #1424 ) ;
#5947 = ADVANCED_FACE ( 'NONE', ( #1004 ), #1181, .F. ) ;
#5948 = CARTESIAN_POINT ( 'NONE',  ( 57.00000000000002132, -1.278008170942866441E-15, 75.00000000000000000 ) ) ;
#5949 = EDGE_CURVE ( 'NONE', #3109, #4600, #4288, .T. ) ;
#5950 = APPLICATION_CONTEXT ( 'automotive_design' ) ;
#5951 = FILL_AREA_STYLE_COLOUR ( '', #1580 ) ;
#5952 = CARTESIAN_POINT ( 'NONE',  ( 25.00000000000000711, 7.000000000000011546, -65.00000000000000000 ) ) ;
#5953 = EDGE_CURVE ( 'NONE', #2345, #5415, #4714, .T. ) ;
#5954 = CYLINDRICAL_SURFACE ( 'NONE', #1446, 5.000000000000000000 ) ;
#5955 = ORIENTED_EDGE ( 'NONE', *, *, #316, .T. ) ;
#5956 = EDGE_LOOP ( 'NONE', ( #4525, #1497, #253, #3285 ) ) ;
#5957 = DIRECTION ( 'NONE',  ( -0.000000000000000000, -1.000000000000000000, -0.000000000000000000 ) ) ;
#5958 = CARTESIAN_POINT ( 'NONE',  ( 55.00000000000000711, -15.00000000000000355, 75.00000000000000000 ) ) ;
#5959 = ORIENTED_EDGE ( 'NONE', *, *, #910, .T. ) ;
#5960 = FACE_OUTER_BOUND ( 'NONE', #22, .T. ) ;
#5961 = ADVANCED_FACE ( 'NONE', ( #100 ), #1935, .F. ) ;
#5962 = DIRECTION ( 'NONE',  ( 0.000000000000000000, 0.000000000000000000, 1.000000000000000000 ) ) ;
#5963 = VERTEX_POINT ( 'NONE', #613 ) ;
#5964 = CARTESIAN_POINT ( 'NONE',  ( 60.00000000000001421, -1.951563910473909559E-15, -55.00000000000000000 ) ) ;
#5965 = ORIENTED_EDGE ( 'NONE', *, *, #3706, .T. ) ;
#5966 = DIRECTION ( 'NONE',  ( -1.000000000000000000, 0.000000000000000000, -0.000000000000000000 ) ) ;
#5967 = CARTESIAN_POINT ( 'NONE',  ( 75.00000000000001421, 0.000000000000000000, 9.500000000000000000 ) ) ;
#5968 = CIRCLE ( 'NONE', #926, 5.000000000000000000 ) ;
#5969 = CARTESIAN_POINT ( 'NONE',  ( 37.50000000000000711, 6.288372600415927295E-15, 65.00000000000000000 ) ) ;
#5970 = CARTESIAN_POINT ( 'NONE',  ( 75.00000000000001421, 0.000000000000000000, -7.000000000000000000 ) ) ;
#5971 = CARTESIAN_POINT ( 'NONE',  ( 75.00000000000001421, -15.00000000000000355, 75.00000000000000000 ) ) ;
#5972 = NEXT_ASSEMBLY_USAGE_OCCURRENCE ( 'NAUO1', ' ', ' ', #3543, #5537, $ ) ;
#5973 = NEXT_ASSEMBLY_USAGE_OCCURRENCE ( 'NAUO2', ' ', ' ', #3543, #2413, $ ) ;
#5974 = NEXT_ASSEMBLY_USAGE_OCCURRENCE ( 'NAUO3', ' ', ' ', #3543, #3494, $ ) ;
#5975 = NEXT_ASSEMBLY_USAGE_OCCURRENCE ( 'NAUO4', ' ', ' ', #3543, #791, $ ) ;
#5976 = NEXT_ASSEMBLY_USAGE_OCCURRENCE ( 'NAUO5', ' ', ' ', #3543, #3383, $ ) ;
#5977 = NEXT_ASSEMBLY_USAGE_OCCURRENCE ( 'NAUO6', ' ', ' ', #3543, #3939, $ ) ;
#5978 = NEXT_ASSEMBLY_USAGE_OCCURRENCE ( 'NAUO7', ' ', ' ', #3543, #2570, $ ) ;
#5979 = NEXT_ASSEMBLY_USAGE_OCCURRENCE ( 'NAUO8', ' ', ' ', #3543, #3311, $ ) ;
#5980 = NEXT_ASSEMBLY_USAGE_OCCURRENCE ( 'NAUO9', ' ', ' ', #3543, #3494, $ ) ;
#5981 = NEXT_ASSEMBLY_USAGE_OCCURRENCE ( 'NAUO10', ' ', ' ', #3543, #2413, $ ) ;
#5982 = NEXT_ASSEMBLY_USAGE_OCCURRENCE ( 'NAUO11', ' ', ' ', #3543, #3383, $ ) ;
#5983 = NEXT_ASSEMBLY_USAGE_OCCURRENCE ( 'NAUO12', ' ', ' ', #3543, #3494, $ ) ;
#5984 = NEXT_ASSEMBLY_USAGE_OCCURRENCE ( 'NAUO13', ' ', ' ', #3543, #3383, $ ) ;
#5985 = NEXT_ASSEMBLY_USAGE_OCCURRENCE ( 'NAUO14', ' ', ' ', #3543, #791, $ ) ;
#5986 = NEXT_ASSEMBLY_USAGE_OCCURRENCE ( 'NAUO15', ' ', ' ', #3543, #2280, $ ) ;
#5987 = NEXT_ASSEMBLY_USAGE_OCCURRENCE ( 'NAUO16', ' ', ' ', #3543, #2280, $ ) ;
#5988 = NEXT_ASSEMBLY_USAGE_OCCURRENCE ( 'NAUO17', ' ', ' ', #3543, #3383, $ ) ;
#5989 = NEXT_ASSEMBLY_USAGE_OCCURRENCE ( 'NAUO18', ' ', ' ', #3543, #3494, $ ) ;
#5990 = NEXT_ASSEMBLY_USAGE_OCCURRENCE ( 'NAUO19', ' ', ' ', #3543, #4803, $ ) ;
#5991 = NEXT_ASSEMBLY_USAGE_OCCURRENCE ( 'NAUO20', ' ', ' ', #3543, #4803, $ ) ;
#5992 = NEXT_ASSEMBLY_USAGE_OCCURRENCE ( 'NAUO21', ' ', ' ', #3543, #3383, $ ) ;
#5993=COLOUR_RGB('Dark Blue',0.08,0.2,0.34);
#5994=FILL_AREA_STYLE_COLOUR('',#5993);
#5995=FILL_AREA_STYLE('',(#5994));
#5996=SURFACE_STYLE_FILL_AREA(#5995);
#5997=SURFACE_SIDE_STYLE('',(#5996));
#5998=SURFACE_STYLE_USAGE(.BOTH.,#5997);
#5999=PRESENTATION_STYLE_ASSIGNMENT((#5998));
#6000=COLOUR_RGB('Light Blue',0.38,0.62,0.78);
#6001=FILL_AREA_STYLE_COLOUR('',#6000);
#6002=FILL_AREA_STYLE('',(#6001));
#6003=SURFACE_STYLE_FILL_AREA(#6002);
#6004=SURFACE_SIDE_STYLE('',(#6003));
#6005=SURFACE_STYLE_USAGE(.BOTH.,#6004);
#6006=PRESENTATION_STYLE_ASSIGNMENT((#6005));
#6007=COLOUR_RGB('Sky Blue',0.24,0.69,0.87);
#6008=FILL_AREA_STYLE_COLOUR('',#6007);
#6009=FILL_AREA_STYLE('',(#6008));
#6010=SURFACE_STYLE_FILL_AREA(#6009);
#6011=SURFACE_SIDE_STYLE('',(#6010));
#6012=SURFACE_STYLE_USAGE(.BOTH.,#6011);
#6013=PRESENTATION_STYLE_ASSIGNMENT((#6012));
#6014=COLOUR_RGB('Grey',0.48,0.52,0.57);
#6015=FILL_AREA_STYLE_COLOUR('',#6014);
#6016=FILL_AREA_STYLE('',(#6015));
#6017=SURFACE_STYLE_FILL_AREA(#6016);
#6018=SURFACE_SIDE_STYLE('',(#6017));
#6019=SURFACE_STYLE_USAGE(.BOTH.,#6018);
#6020=PRESENTATION_STYLE_ASSIGNMENT((#6019));
#6021=COLOUR_RGB('Black',0.12,0.14,0.17);
#6022=FILL_AREA_STYLE_COLOUR('',#6021);
#6023=FILL_AREA_STYLE('',(#6022));
#6024=SURFACE_STYLE_FILL_AREA(#6023);
#6025=SURFACE_SIDE_STYLE('',(#6024));
#6026=SURFACE_STYLE_USAGE(.BOTH.,#6025);
#6027=PRESENTATION_STYLE_ASSIGNMENT((#6026));
#6028=COLOUR_RGB('Off White',0.89,0.88,0.83);
#6029=FILL_AREA_STYLE_COLOUR('',#6028);
#6030=FILL_AREA_STYLE('',(#6029));
#6031=SURFACE_STYLE_FILL_AREA(#6030);
#6032=SURFACE_SIDE_STYLE('',(#6031));
#6033=SURFACE_STYLE_USAGE(.BOTH.,#6032);
#6034=PRESENTATION_STYLE_ASSIGNMENT((#6033));
ENDSEC;
END-ISO-10303-21;
